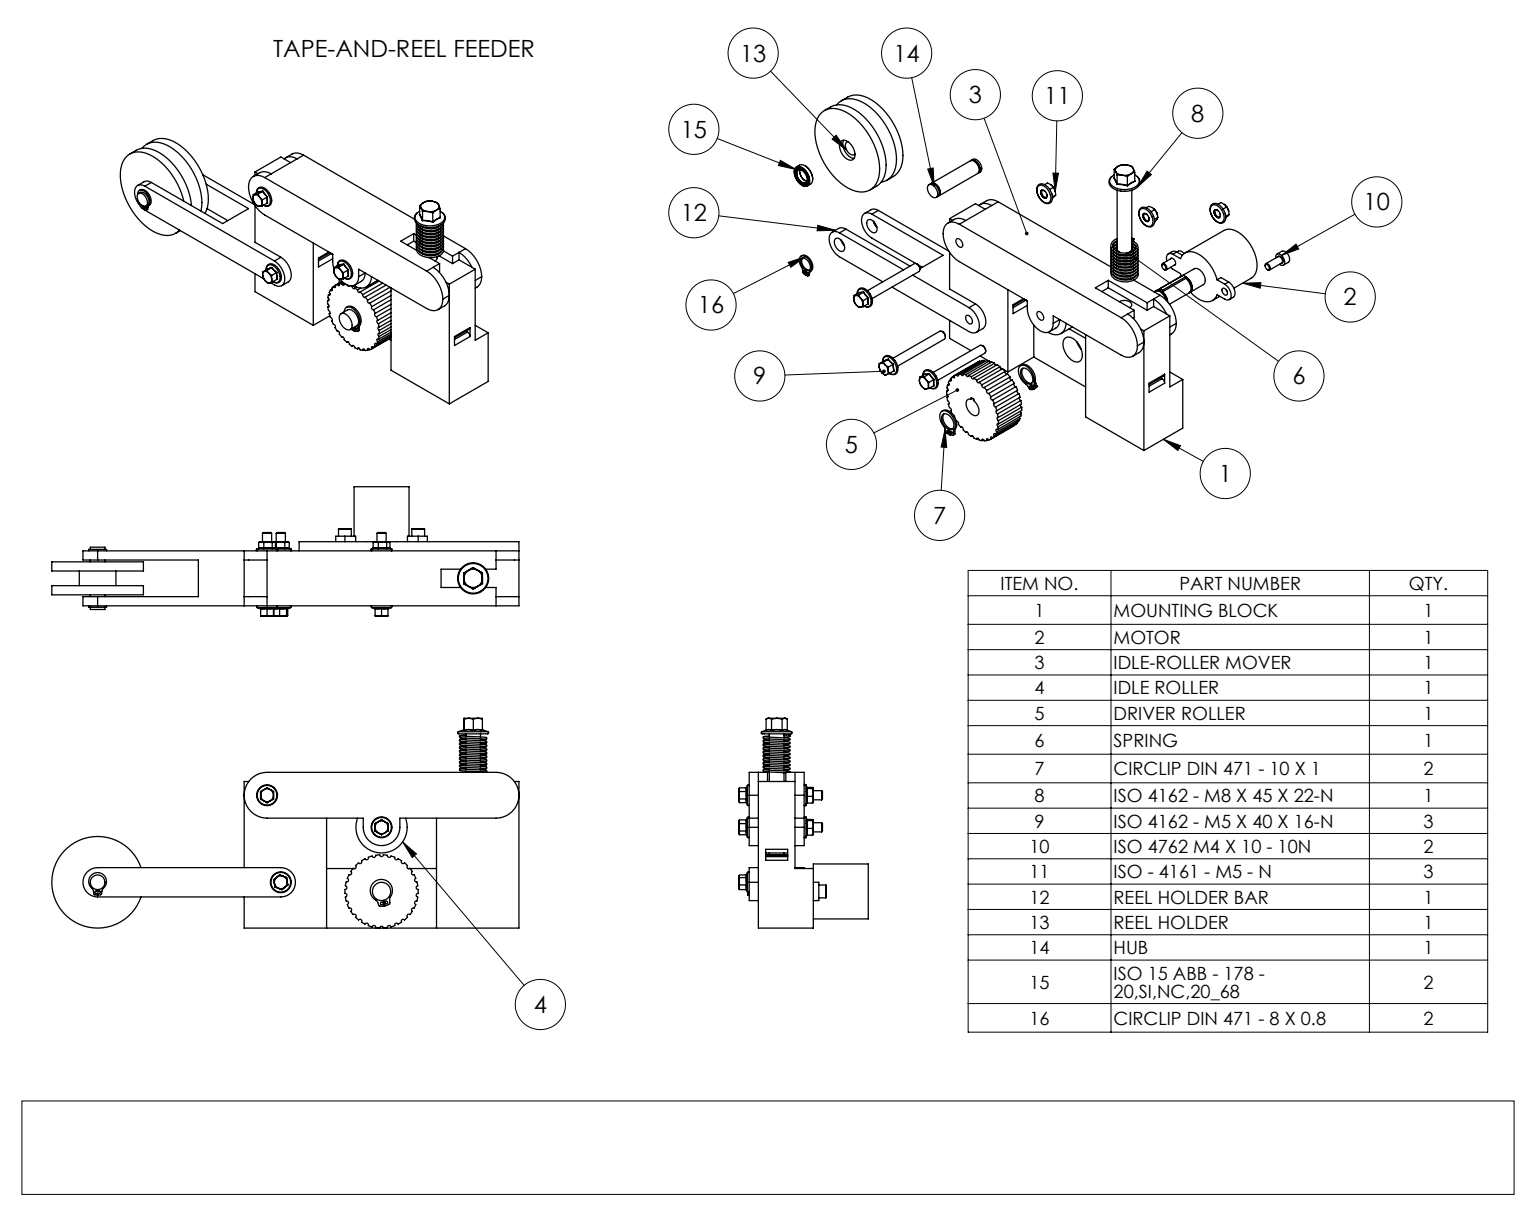
ISO-10303-21;
HEADER;
FILE_DESCRIPTION (('STEP AP214'),
    '1' );
FILE_NAME ('MAS-177',
    '2026-10-31T03:44:21',
    ( '' ),
    ( '' ),
    'SwSTEP 2.0',
    'SolidWorks 2026',
    '' );
FILE_SCHEMA (( 'AUTOMOTIVE_DESIGN' ));
ENDSEC;

DATA;
#1 = CARTESIAN_POINT ( 'NONE',  ( 55.94051828345054389, 59.20051614449765509, 4.345558710429044957 ) ) ;
#2 = ORIENTED_EDGE ( 'NONE', *, *, #6633, .F. ) ;
#3 = DIRECTION ( 'NONE',  ( -0.9999670257950099561, -0.008120795692649453515, 0.000000000000000000 ) ) ;
#4 = CARTESIAN_POINT ( 'NONE',  ( 3.972066048304701891, -2.740530939476090388, 2.384802634787825504 ) ) ;
#5 = CARTESIAN_POINT ( 'NONE',  ( 55.08986747509849380, 53.20051614449766220, 3.727524721679155384 ) ) ;
#6 = CARTESIAN_POINT ( 'NONE',  ( -154.9999999999999716, -14.99999999999999645, 15.00000000000000000 ) ) ;
#7 = CARTESIAN_POINT ( 'NONE',  ( 55.11794222512601493, 60.19948385550240744, 3.688883143319541702 ) ) ;
#8 = DIRECTION ( 'NONE',  ( 0.000000000000000000, 0.000000000000000000, 1.000000000000000000 ) ) ;
#9 = CARTESIAN_POINT ( 'NONE',  ( 44.05948171654949874, 50.79948385550238754, 4.345558710429105354 ) ) ;
#10 = VECTOR ( 'NONE', #15032, 1000.000000000000000 ) ;
#11 = CARTESIAN_POINT ( 'NONE',  ( 43.18075615816994173, 53.80051614449766362, 4.924951120819380357 ) ) ;
#12 = CARTESIAN_POINT ( 'NONE',  ( 6.204460410672268722, -3.831267809382561840, 3.364049496746113199 ) ) ;
#13 = CARTESIAN_POINT ( 'NONE',  ( -57.64999999999994884, -14.99999999999998579, -10.00000000000000178 ) ) ;
#14 = DIRECTION ( 'NONE',  ( -4.082155997157844188E-16, 1.000000000000000000, 0.000000000000000000 ) ) ;
#15 = SURFACE_STYLE_USAGE ( .BOTH. , #11569 ) ;
#16 = SHAPE_DEFINITION_REPRESENTATION ( #10384, #4039 ) ;
#17 = AXIS2_PLACEMENT_3D ( 'NONE', #16816, #16917, #3571 ) ;
#18 = EDGE_LOOP ( 'NONE', ( #11625, #15008, #6307, #1224 ) ) ;
#19 = CARTESIAN_POINT ( 'NONE',  ( 0.000000000000000000, -3.031088913245534755, -1.750000000000001332 ) ) ;
#20 = LINE ( 'NONE', #7849, #12198 ) ;
#21 =( REPRESENTATION_RELATIONSHIP ('NONE','NONE', #16703, #13428 ) REPRESENTATION_RELATIONSHIP_WITH_TRANSFORMATION ( #8023 )SHAPE_REPRESENTATION_RELATIONSHIP( ) );
#22 = AXIS2_PLACEMENT_3D ( 'NONE', #10156, #1151, #17072 ) ;
#23 = CARTESIAN_POINT ( 'NONE',  ( 50.02271294988512551, 62.49948385550240459, 7.000000000000000888 ) ) ;
#24 = VECTOR ( 'NONE', #9487, 1000.000000000000000 ) ;
#25 = CARTESIAN_POINT ( 'NONE',  ( 5.000000000000003553, -20.00000000000000000, 9.999999999999998224 ) ) ;
#26 = CIRCLE ( 'NONE', #5977, 1.999999999999998224 ) ;
#27 = DIRECTION ( 'NONE',  ( -0.000000000000000000, -0.000000000000000000, -1.000000000000000000 ) ) ;
#28 = FACE_OUTER_BOUND ( 'NONE', #18793, .T. ) ;
#29 = CARTESIAN_POINT ( 'NONE',  ( 47.74827507625478518, 56.59948385550238470, 7.007379884777227730 ) ) ;
#30 = CIRCLE ( 'NONE', #4409, 4.100000000000000533 ) ;
#31 = DIRECTION ( 'NONE',  ( -0.000000000000000000, 1.000000000000000000, -0.000000000000000000 ) ) ;
#32 = CARTESIAN_POINT ( 'NONE',  ( 54.68390685589033495, 51.69948385550241454, -6.485486291978119766 ) ) ;
#33 = CARTESIAN_POINT ( 'NONE',  ( 1.150000000000001688, 7.347880794884120722E-16, 6.000000000000000888 ) ) ;
#34 = CARTESIAN_POINT ( 'NONE',  ( 56.65037692655921120, 57.10051614449766078, 2.184720259617097593 ) ) ;
#35 = DIRECTION ( 'NONE',  ( -1.000000000000000000, 0.000000000000000000, 0.000000000000000000 ) ) ;
#36 = ORIENTED_EDGE ( 'NONE', *, *, #18632, .T. ) ;
#37 =( NAMED_UNIT ( * ) PLANE_ANGLE_UNIT ( ) SI_UNIT ( $, .RADIAN. ) );
#38 = VECTOR ( 'NONE', #9468, 1000.000000000000000 ) ;
#39 = AXIS2_PLACEMENT_3D ( 'NONE', #18626, #14180, #9573 ) ;
#40 = VERTEX_POINT ( 'NONE', #10112 ) ;
#41 = AXIS2_PLACEMENT_3D ( 'NONE', #5038, #18489, #12385 ) ;
#42 = CARTESIAN_POINT ( 'NONE',  ( 13.99999999999999822, 0.000000000000000000, 0.000000000000000000 ) ) ;
#43 = ORIENTED_EDGE ( 'NONE', *, *, #11589, .T. ) ;
#44 = CYLINDRICAL_SURFACE ( 'NONE', #13500, 4.799999999999999822 ) ;
#45 = ORIENTED_EDGE ( 'NONE', *, *, #3522, .F. ) ;
#46 = CARTESIAN_POINT ( 'NONE',  ( 2.000000000000005329, -3.464101615137751722, 0.000000000000000000 ) ) ;
#47 = ORIENTED_EDGE ( 'NONE', *, *, #5852, .F. ) ;
#48 = DIRECTION ( 'NONE',  ( 1.000000000000000000, 0.000000000000000000, 0.000000000000000000 ) ) ;
#49 = DIRECTION ( 'NONE',  ( -0.000000000000000000, -0.000000000000000000, -1.000000000000000000 ) ) ;
#50 = EDGE_CURVE ( 'NONE', #8587, #13131, #8250, .T. ) ;
#51 = CARTESIAN_POINT ( 'NONE',  ( 44.28664221472220675, 59.09948385550240602, -1.832500667257165317 ) ) ;
#52 = CARTESIAN_POINT ( 'NONE',  ( -2.000000000000006661, 3.464101615137750834, 0.000000000000000000 ) ) ;
#53 = DIRECTION ( 'NONE',  ( -1.000000000000000000, 0.000000000000000000, 0.000000000000000000 ) ) ;
#54 = VECTOR ( 'NONE', #3678, 1000.000000000000000 ) ;
#55 = CIRCLE ( 'NONE', #4760, 5.000000000000000888 ) ;
#56 = CARTESIAN_POINT ( 'NONE',  ( 49.97728705011495265, 51.50051614449765935, 8.000000000000001776 ) ) ;
#57 = CARTESIAN_POINT ( 'NONE',  ( 53.54508667620424234, 58.70051614449765509, -4.840751629271188961 ) ) ;
#58 = EDGE_CURVE ( 'NONE', #17997, #75, #9295, .T. ) ;
#59 = AXIS2_PLACEMENT_3D ( 'NONE', #5322, #457, #13965 ) ;
#60 = FACE_OUTER_BOUND ( 'NONE', #12914, .T. ) ;
#61 = FACE_OUTER_BOUND ( 'NONE', #9370, .T. ) ;
#62 = VERTEX_POINT ( 'NONE', #14718 ) ;
#63 = ADVANCED_FACE ( 'NONE', ( #9131 ), #4633, .F. ) ;
#64 = ADVANCED_FACE ( 'NONE', ( #5901 ), #7658, .T. ) ;
#65 = ORIENTED_EDGE ( 'NONE', *, *, #19121, .F. ) ;
#66 = DIRECTION ( 'NONE',  ( -1.000000000000000000, 0.000000000000000000, 0.000000000000000000 ) ) ;
#67 = ORIENTED_EDGE ( 'NONE', *, *, #8672, .F. ) ;
#68 = ADVANCED_FACE ( 'NONE', ( #1306 ), #2882, .T. ) ;
#69 = CARTESIAN_POINT ( 'NONE',  ( 44.05948171654949874, 62.79948385550241596, 4.345558710429105354 ) ) ;
#70 = DIRECTION ( 'NONE',  ( -0.9989677110047504582, -0.04542589977017007230, 1.386346192018204258E-14 ) ) ;
#71 = VERTEX_POINT ( 'NONE', #1398 ) ;
#72 = DIRECTION ( 'NONE',  ( -0.000000000000000000, -0.000000000000000000, 1.000000000000000000 ) ) ;
#73 = CARTESIAN_POINT ( 'NONE',  ( 0.9183817310753816798, -24.91493387504114665, 15.00000000000000355 ) ) ;
#74 = CIRCLE ( 'NONE', #18561, 24.99999999999999289 ) ;
#75 = VERTEX_POINT ( 'NONE', #7374 ) ;
#76 = EDGE_LOOP ( 'NONE', ( #8568, #3625 ) ) ;
#77 = CARTESIAN_POINT ( 'NONE',  ( 58.41169779390614281, 45.99948385550240459, -0.02388180880523160798 ) ) ;
#78 = CARTESIAN_POINT ( 'NONE',  ( -62.49999999999997158, 32.50000000000001421, 15.00000000000000000 ) ) ;
#79 = EDGE_CURVE ( 'NONE', #3064, #8689, #14380, .T. ) ;
#80 = CARTESIAN_POINT ( 'NONE',  ( 50.02271294988512551, 56.49948385550240459, 7.000000000000000888 ) ) ;
#81 = FACE_OUTER_BOUND ( 'NONE', #5769, .T. ) ;
#82 = EDGE_CURVE ( 'NONE', #6843, #7000, #17682, .T. ) ;
#83 = CARTESIAN_POINT ( 'NONE',  ( 4.000000000000000000, -2.309401076758516691, -0.4999999999999995559 ) ) ;
#84 = CARTESIAN_POINT ( 'NONE',  ( 43.34962307344078880, 54.10051614449766788, -2.184720259617096705 ) ) ;
#85 = LINE ( 'NONE', #5764, #17678 ) ;
#86 = SURFACE_STYLE_FILL_AREA ( #10453 ) ;
#87 = CARTESIAN_POINT ( 'NONE',  ( -155.0676494111543491, -18.79939778875158396, -15.79999999999999893 ) ) ;
#88 = VERTEX_POINT ( 'NONE', #4235 ) ;
#89 = ORIENTED_EDGE ( 'NONE', *, *, #4960, .T. ) ;
#90 = ORIENTED_EDGE ( 'NONE', *, *, #9609, .F. ) ;
#91 = CARTESIAN_POINT ( 'NONE',  ( 0.000000000000000000, -4.330127018922193649, -2.500000000000000000 ) ) ;
#92 = CARTESIAN_POINT ( 'NONE',  ( 43.20883090819745576, 64.79948385550240175, 4.963592699179006473 ) ) ;
#93 = DIRECTION ( 'NONE',  ( 0.000000000000000000, 0.000000000000000000, -1.000000000000000000 ) ) ;
#94 = EDGE_LOOP ( 'NONE', ( #13981, #857, #13951, #13577 ) ) ;
#95 = DIRECTION ( 'NONE',  ( -1.000000000000000000, 0.000000000000000000, 0.000000000000000000 ) ) ;
#96 = ORIENTED_EDGE ( 'NONE', *, *, #2338, .F. ) ;
#97 = CARTESIAN_POINT ( 'NONE',  ( 42.63976443033212149, 62.00051614449765225, -0.02388180880514948964 ) ) ;
#98 = EDGE_LOOP ( 'NONE', ( #16825, #4410, #16982, #5745 ) ) ;
#99 = DIRECTION ( 'NONE',  ( -1.000000000000000000, 0.000000000000000000, -0.000000000000000000 ) ) ;
#100 = UNCERTAINTY_MEASURE_WITH_UNIT (LENGTH_MEASURE( 1.000000000000000082E-05 ), #14123, 'distance_accuracy_value', 'NONE');
#101 = CARTESIAN_POINT ( 'NONE',  ( -74.99999999999997158, 1.000000000000000000, -5.999999999999998224 ) ) ;
#102 = EDGE_CURVE ( 'NONE', #16449, #12595, #15014, .T. ) ;
#103 = CARTESIAN_POINT ( 'NONE',  ( 55.11794222512599362, 56.80051614449764941, -3.688883143319583446 ) ) ;
#104 = CARTESIAN_POINT ( 'NONE',  ( -62.49999999999997158, 32.50000000000001421, -15.00000000000000000 ) ) ;
#105 = ADVANCED_FACE ( 'NONE', ( #13344 ), #11768, .F. ) ;
#106 = CARTESIAN_POINT ( 'NONE',  ( 49.97728705011488870, 55.49948385550241170, -6.000000000000000888 ) ) ;
#107 = FACE_OUTER_BOUND ( 'NONE', #1049, .T. ) ;
#108 = CARTESIAN_POINT ( 'NONE',  ( 43.20883090819742023, 54.20051614449766220, -4.963592699178938972 ) ) ;
#109 = CARTESIAN_POINT ( 'NONE',  ( 5.991014884144049368, -4.330127018922197202, -2.500000000000000444 ) ) ;
#110 = CARTESIAN_POINT ( 'NONE',  ( 3.961551342853669944, 3.742715940867779700, -0.5174258321190529086 ) ) ;
#111 = ORIENTED_EDGE ( 'NONE', *, *, #1854, .F. ) ;
#112 = CARTESIAN_POINT ( 'NONE',  ( 8.500000000000000000, 0.000000000000000000, 7.900000000000002132 ) ) ;
#113 =( NAMED_UNIT ( * ) SI_UNIT ( $, .STERADIAN. ) SOLID_ANGLE_UNIT ( ) );
#114 = ORIENTED_EDGE ( 'NONE', *, *, #10804, .F. ) ;
#115 = CARTESIAN_POINT ( 'NONE',  ( 0.000000000000000000, 0.000000000000000000, 0.000000000000000000 ) ) ;
#116 = EDGE_CURVE ( 'NONE', #14983, #12413, #19360, .T. ) ;
#117 = DIRECTION ( 'NONE',  ( 0.000000000000000000, 0.000000000000000000, 1.000000000000000000 ) ) ;
#118 = EDGE_CURVE ( 'NONE', #2113, #2665, #16595, .T. ) ;
#119 = CARTESIAN_POINT ( 'NONE',  ( 43.33558569842703179, 65.09948385550239891, -2.141517661632099223 ) ) ;
#120 = CARTESIAN_POINT ( 'NONE',  ( 6.534533895392294234, 2.951347675328725106, 5.111884124469659341 ) ) ;
#121 = CARTESIAN_POINT ( 'NONE',  ( -0.9999999999999995559, -15.10102051443364246, 9.000000000000000000 ) ) ;
#122 = DIRECTION ( 'NONE',  ( -1.000000000000000000, 0.000000000000000000, 0.000000000000000000 ) ) ;
#123 = CARTESIAN_POINT ( 'NONE',  ( 44.03140696652192787, 61.19948385550239323, -4.306917132069425058 ) ) ;
#124 = CARTESIAN_POINT ( 'NONE',  ( 1.411581201560190495E-15, 4.862606272033091592, -3.745885042887436622 ) ) ;
#125 = CARTESIAN_POINT ( 'NONE',  ( 43.18075615816989199, 53.19948385550240744, -4.924951120819313743 ) ) ;
#126 = DIRECTION ( 'NONE',  ( -0.000000000000000000, -0.000000000000000000, -1.000000000000000000 ) ) ;
#127 = CARTESIAN_POINT ( 'NONE',  ( 45.90387839640208512, 54.30051614449765651, -5.676469297603124353 ) ) ;
#128 = DIRECTION ( 'NONE',  ( 0.000000000000000000, -0.000000000000000000, 1.000000000000000000 ) ) ;
#129 = ORIENTED_EDGE ( 'NONE', *, *, #17684, .F. ) ;
#130 = AXIS2_PLACEMENT_3D ( 'NONE', #17222, #3785, #15743 ) ;
#131 = ORIENTED_EDGE ( 'NONE', *, *, #8892, .F. ) ;
#132 = AXIS2_PLACEMENT_3D ( 'NONE', #16115, #16207, #5718 ) ;
#133 = CARTESIAN_POINT ( 'NONE',  ( 6.527192678185834929, 2.941622124011056272, -5.095038975456026797 ) ) ;
#134 = ORIENTED_EDGE ( 'NONE', *, *, #5000, .T. ) ;
#135 = DIRECTION ( 'NONE',  ( -9.710251638871371392E-17, -5.969973981896233748E-17, -1.000000000000000000 ) ) ;
#136 = CARTESIAN_POINT ( 'NONE',  ( 55.96859303347804371, 62.19948385550240744, 4.306917132069425946 ) ) ;
#137 = PLANE ( 'NONE',  #4619 ) ;
#138 = ORIENTED_EDGE ( 'NONE', *, *, #15996, .F. ) ;
#139 = CARTESIAN_POINT ( 'NONE',  ( -0.2500000000000000000, -8.096141056083446585, -1.000000000000000000 ) ) ;
#140 = LINE ( 'NONE', #4756, #15155 ) ;
#141 = CARTESIAN_POINT ( 'NONE',  ( 51.97223112728254790, 58.39948385550241028, 5.992620115222778487 ) ) ;
#142 = DIRECTION ( 'NONE',  ( -0.9781476007338065770, 0.2079116908177552348, 0.000000000000000000 ) ) ;
#143 = DIRECTION ( 'NONE',  ( -0.000000000000000000, -0.000000000000000000, -1.000000000000000000 ) ) ;
#144 = CARTESIAN_POINT ( 'NONE',  ( 45.31609314410960820, 54.30051614449765651, -6.485486291978072693 ) ) ;
#145 = CIRCLE ( 'NONE', #8274, 20.00000000000000000 ) ;
#146 = CARTESIAN_POINT ( 'NONE',  ( 48.07319477248762496, 54.40051614449765793, -6.007379884777208190 ) ) ;
#147 = B_SPLINE_CURVE_WITH_KNOTS ( 'NONE', 3,
 ( #14538, #3778, #12976, #8661, #17507, #4068 ),
 .UNSPECIFIED., .F., .F.,
 ( 4, 2, 4 ),
 ( 0.000000000000000000, 0.0002095117440854730670, 0.0004190234881709461339 ),
 .UNSPECIFIED. ) ;
#148 = CARTESIAN_POINT ( 'NONE',  ( -0.2000000000000000111, -6.997142273814360713, -0.8000000000000000444 ) ) ;
#149 = DIRECTION ( 'NONE',  ( -0.6520673188974834833, 0.7581610723493047432, 1.805535875966851803E-17 ) ) ;
#150 = ORIENTED_EDGE ( 'NONE', *, *, #5080, .F. ) ;
#151 = ORIENTED_EDGE ( 'NONE', *, *, #16122, .F. ) ;
#152 = CARTESIAN_POINT ( 'NONE',  ( 11.75570504584926468, -3.819660112500910198, 9.000000000000000000 ) ) ;
#153 = VERTEX_POINT ( 'NONE', #25 ) ;
#154 = ADVANCED_FACE ( 'NONE', ( #6013 ), #15557, .T. ) ;
#155 = CARTESIAN_POINT ( 'NONE',  ( 54.09612160359786515, 63.69948385550240744, -5.676469297603166098 ) ) ;
#156 = CARTESIAN_POINT ( 'NONE',  ( -99.99999999999997158, -23.00000000000000711, 15.00000000000000000 ) ) ;
#157 = ORIENTED_EDGE ( 'NONE', *, *, #5820, .T. ) ;
#158 = AXIS2_PLACEMENT_3D ( 'NONE', #16967, #16677, #18346 ) ;
#159 = DIRECTION ( 'NONE',  ( 1.000000000000000000, 0.000000000000000000, 0.000000000000000000 ) ) ;
#160 = PRODUCT_DEFINITION ( 'UNKNOWN', '', #4804, #10473 ) ;
#161 = DIRECTION ( 'NONE',  ( 0.000000000000000000, 0.000000000000000000, 1.000000000000000000 ) ) ;
#162 = VERTEX_POINT ( 'NONE', #1595 ) ;
#163 = DIRECTION ( 'NONE',  ( -0.9999670257950099561, -0.008120795692649453515, 0.000000000000000000 ) ) ;
#164 = VERTEX_POINT ( 'NONE', #8741 ) ;
#165 = CARTESIAN_POINT ( 'NONE',  ( 47.37792948025162332, 47.39948385550241028, -7.992620115222770494 ) ) ;
#166 = CARTESIAN_POINT ( 'NONE',  ( 2.899426713160750069, -23.82535289025860337, -8.999999999999996447 ) ) ;
#167 = EDGE_CURVE ( 'NONE', #12421, #12590, #7736, .T. ) ;
#168 = EDGE_CURVE ( 'NONE', #12513, #18552, #6292, .T. ) ;
#169 = CARTESIAN_POINT ( 'NONE',  ( 55.94051828345050836, 55.79948385550238044, -4.345558710429104465 ) ) ;
#170 = DIRECTION ( 'NONE',  ( 0.000000000000000000, -1.000000000000000000, -0.000000000000000000 ) ) ;
#171 = DIRECTION ( 'NONE',  ( -0.000000000000000000, -0.000000000000000000, -1.000000000000000000 ) ) ;
#172 = CARTESIAN_POINT ( 'NONE',  ( 56.66441430157294690, 56.90051614449766504, -2.141517661632166281 ) ) ;
#173 = CARTESIAN_POINT ( 'NONE',  ( 0.000000000000000000, 0.000000000000000000, -0.8000000000000000444 ) ) ;
#174 = ADVANCED_FACE ( 'NONE', ( #9593 ), #15208, .F. ) ;
#175 = DIRECTION ( 'NONE',  ( 1.000000000000000000, 0.000000000000000000, 0.000000000000000000 ) ) ;
#176 = EDGE_CURVE ( 'NONE', #16215, #3087, #11160, .T. ) ;
#177 = DIRECTION ( 'NONE',  ( 0.000000000000000000, 0.000000000000000000, 1.000000000000000000 ) ) ;
#178 = VERTEX_POINT ( 'NONE', #10980 ) ;
#179 = ORIENTED_EDGE ( 'NONE', *, *, #18456, .F. ) ;
#180 = ORIENTED_EDGE ( 'NONE', *, *, #9393, .F. ) ;
#181 = DIRECTION ( 'NONE',  ( 1.000000000000000000, 0.000000000000000000, 0.000000000000000000 ) ) ;
#182 = SURFACE_STYLE_USAGE ( .BOTH. , #380 ) ;
#183 = CIRCLE ( 'NONE', #15507, 5.000000000000000888 ) ;
#184 = EDGE_CURVE ( 'NONE', #2510, #7366, #17139, .T. ) ;
#185 = CARTESIAN_POINT ( 'NONE',  ( 57.61547081786812896, 64.09948385550239891, 2.450534656007040901 ) ) ;
#186 = EDGE_CURVE ( 'NONE', #9539, #16928, #1996, .T. ) ;
#187 = ORIENTED_EDGE ( 'NONE', *, *, #1986, .T. ) ;
#188 = CARTESIAN_POINT ( 'NONE',  ( -20.63749999999999574, 0.000000000000000000, 0.000000000000000000 ) ) ;
#189 = VERTEX_POINT ( 'NONE', #16887 ) ;
#190 = CARTESIAN_POINT ( 'NONE',  ( 44.05948171654945611, 58.20051614449764799, -4.345558710429044069 ) ) ;
#191 = ORIENTED_EDGE ( 'NONE', *, *, #16975, .F. ) ;
#192 = ADVANCED_FACE ( 'NONE', ( #13732 ), #15592, .F. ) ;
#193 = CARTESIAN_POINT ( 'NONE',  ( -3.158233816355059620, -39.56295201467614220, -9.000000000000000000 ) ) ;
#194 = DIRECTION ( 'NONE',  ( -1.000000000000000000, -0.000000000000000000, -0.000000000000000000 ) ) ;
#195 = EDGE_CURVE ( 'NONE', #14529, #9351, #3542, .T. ) ;
#196 = CARTESIAN_POINT ( 'NONE',  ( 50.02271294988506156, 56.50051614449767357, -6.000000000000000888 ) ) ;
#197 = CARTESIAN_POINT ( 'NONE',  ( 0.000000000000000000, 4.163799117101000559E-16, -3.299999999999999822 ) ) ;
#198 = CIRCLE ( 'NONE', #9874, 1.000000000000000000 ) ;
#199 = CARTESIAN_POINT ( 'NONE',  ( -19.30627432446647163, -14.77814480204146363, 9.000000000000000000 ) ) ;
#200 = CARTESIAN_POINT ( 'NONE',  ( 46.49166364869460466, 56.69948385550240744, 4.867452303228209765 ) ) ;
#201 = CARTESIAN_POINT ( 'NONE',  ( 2.000000000000000000, 1.773042676681340524, -2.059984127722458425E-15 ) ) ;
#202 = CARTESIAN_POINT ( 'NONE',  ( 47.37792948025170858, 53.60051614449765367, 7.992620115222797139 ) ) ;
#203 = DIRECTION ( 'NONE',  ( -0.000000000000000000, -0.000000000000000000, 1.000000000000000000 ) ) ;
#204 = CARTESIAN_POINT ( 'NONE',  ( -4.204015924366189871, 1.626724848190922446, -3.610627190413390419 ) ) ;
#205 = AXIS2_PLACEMENT_3D ( 'NONE', #2952, #1472, #19344 ) ;
#206 = VERTEX_POINT ( 'NONE', #16694 ) ;
#207 = CARTESIAN_POINT ( 'NONE',  ( 5.599999999999999645, 0.000000000000000000, 0.000000000000000000 ) ) ;
#208 = APPLICATION_PROTOCOL_DEFINITION ( 'draft international standard', 'automotive_design', 1998, #2406 ) ;
#209 = ORIENTED_EDGE ( 'NONE', *, *, #14535, .T. ) ;
#210 = CARTESIAN_POINT ( 'NONE',  ( -1.398397006336996817, -6.091550361990593743, -0.8000000000000000444 ) ) ;
#211 = DIRECTION ( 'NONE',  ( -0.000000000000000000, -0.000000000000000000, 1.000000000000000000 ) ) ;
#212 = CARTESIAN_POINT ( 'NONE',  ( 55.96859303347805081, 62.19948385550241454, 4.306917132069425058 ) ) ;
#213 = DIRECTION ( 'NONE',  ( -1.000000000000000000, -0.000000000000000000, 0.000000000000000000 ) ) ;
#214 = DIRECTION ( 'NONE',  ( -0.000000000000000000, 0.000000000000000000, 1.000000000000000000 ) ) ;
#215 = CYLINDRICAL_SURFACE ( 'NONE', #17154, 2.447112362156698140 ) ;
#216 = CARTESIAN_POINT ( 'NONE',  ( 56.65037692655918988, 57.89948385550240317, -2.184720259617163762 ) ) ;
#217 = DIRECTION ( 'NONE',  ( 0.000000000000000000, 0.000000000000000000, 1.000000000000000000 ) ) ;
#218 = CIRCLE ( 'NONE', #11155, 4.799999999999999822 ) ;
#219 = CARTESIAN_POINT ( 'NONE',  ( 52.57664461997811856, 55.59948385550240602, -8.007379884777229506 ) ) ;
#220 = DIRECTION ( 'NONE',  ( 0.000000000000000000, 0.000000000000000000, -1.000000000000000000 ) ) ;
#221 = CARTESIAN_POINT ( 'NONE',  ( 47.74827507625469281, 54.40051614449766504, -7.007379884777203749 ) ) ;
#222 = EDGE_CURVE ( 'NONE', #2993, #6110, #13306, .T. ) ;
#223 = DIRECTION ( 'NONE',  ( 2.191393683118470056E-17, 7.538405132783724027E-17, 1.000000000000000000 ) ) ;
#224 = ADVANCED_FACE ( 'NONE', ( #6567 ), #9413, .T. ) ;
#225 = ORIENTED_EDGE ( 'NONE', *, *, #17454, .F. ) ;
#226 = VECTOR ( 'NONE', #4356, 1000.000000000000000 ) ;
#227 = DIRECTION ( 'NONE',  ( 0.000000000000000000, -0.000000000000000000, 1.000000000000000000 ) ) ;
#228 = VERTEX_POINT ( 'NONE', #12449 ) ;
#229 = CARTESIAN_POINT ( 'NONE',  ( 57.36023556966787851, 49.00051614449764514, 0.02388180880515038476 ) ) ;
#230 = CARTESIAN_POINT ( 'NONE',  ( 50.02271294988512551, 62.49948385550240459, 7.000000000000000888 ) ) ;
#231 = DIRECTION ( 'NONE',  ( 1.000000000000000000, 0.000000000000000000, 0.000000000000000000 ) ) ;
#232 = EDGE_LOOP ( 'NONE', ( #13470, #855 ) ) ;
#233 = DIRECTION ( 'NONE',  ( -0.3090169943749528914, 0.9510565162951518658, 0.000000000000000000 ) ) ;
#234 = DIRECTION ( 'NONE',  ( 0.000000000000000000, 0.000000000000000000, 1.000000000000000000 ) ) ;
#235 = CARTESIAN_POINT ( 'NONE',  ( 44.91013252490152752, 56.79948385550240175, 3.727524721679198461 ) ) ;
#236 = PLANE ( 'NONE',  #7905 ) ;
#237 = PRESENTATION_STYLE_ASSIGNMENT (( #8960 ) ) ;
#238 = AXIS2_PLACEMENT_3D ( 'NONE', #6880, #15913, #19069 ) ;
#239 = CARTESIAN_POINT ( 'NONE',  ( 49.97728705011495265, 55.50051614449766646, 8.000000000000001776 ) ) ;
#240 = CARTESIAN_POINT ( 'NONE',  ( 53.50833635130544508, 57.30051614449767072, 4.867452303228181343 ) ) ;
#241 = AXIS2_PLACEMENT_3D ( 'NONE', #17266, #3826, #15783 ) ;
#242 = FACE_OUTER_BOUND ( 'NONE', #17390, .T. ) ;
#243 = VECTOR ( 'NONE', #1548, 1000.000000000000114 ) ;
#244 = CARTESIAN_POINT ( 'NONE',  ( 22.14999999999999858, -20.00000000000000000, -20.00000000000000000 ) ) ;
#245 = ORIENTED_EDGE ( 'NONE', *, *, #9904, .T. ) ;
#246 = ORIENTED_EDGE ( 'NONE', *, *, #5677, .F. ) ;
#247 = CARTESIAN_POINT ( 'NONE',  ( 6.327625087026996553, 2.033113452595566972, -4.999999999998725464 ) ) ;
#248 = VERTEX_POINT ( 'NONE', #13911 ) ;
#249 = DIRECTION ( 'NONE',  ( -9.710251638871371392E-17, -5.969973981896233748E-17, -1.000000000000000000 ) ) ;
#250 = DIRECTION ( 'NONE',  ( 0.000000000000000000, 0.000000000000000000, 1.000000000000000000 ) ) ;
#251 = CIRCLE ( 'NONE', #8059, 3.800000000000000266 ) ;
#252 = ORIENTED_EDGE ( 'NONE', *, *, #14423, .F. ) ;
#253 = DIRECTION ( 'NONE',  ( 1.000000000000000000, 0.000000000000000000, 0.000000000000000000 ) ) ;
#254 = CARTESIAN_POINT ( 'NONE',  ( 55.94051828345050836, 51.79948385550240175, -4.345558710429103577 ) ) ;
#255 = CONICAL_SURFACE ( 'NONE', #13715, 2.055000000000000160, 0.7853981633974400633 ) ;
#256 = ORIENTED_EDGE ( 'NONE', *, *, #7357, .T. ) ;
#257 = DIRECTION ( 'NONE',  ( 0.1836763462126260738, -0.9829867750086873635, -1.521953536530129477E-22 ) ) ;
#258 = VERTEX_POINT ( 'NONE', #12266 ) ;
#259 = CARTESIAN_POINT ( 'NONE',  ( 56.81924384183011512, 48.19948385550240744, 4.924951120819313743 ) ) ;
#260 = CARTESIAN_POINT ( 'NONE',  ( 9.999999999999994671, 20.00000000000001421, -9.999999999999998224 ) ) ;
#261 = CARTESIAN_POINT ( 'NONE',  ( 52.25172492374522903, 57.59948385550241312, -7.007379884777225953 ) ) ;
#262 = CARTESIAN_POINT ( 'NONE',  ( -154.9999999999999716, -14.99999999999999645, 15.79999999999999893 ) ) ;
#263 =( GEOMETRIC_REPRESENTATION_CONTEXT ( 3 ) GLOBAL_UNCERTAINTY_ASSIGNED_CONTEXT ( ( #6357 ) ) GLOBAL_UNIT_ASSIGNED_CONTEXT ( ( #5384, #15479, #3919 ) ) REPRESENTATION_CONTEXT ( 'NONE', 'WORKASPACE' ) );
#264 = CARTESIAN_POINT ( 'NONE',  ( 54.09612160359792199, 57.30051614449765651, 5.676469297603124353 ) ) ;
#265 = EDGE_CURVE ( 'NONE', #12240, #6347, #18266, .T. ) ;
#266 = CYLINDRICAL_SURFACE ( 'NONE', #9428, 5.999999999999977796 ) ;
#267 = CARTESIAN_POINT ( 'NONE',  ( 6.452281807715811723, -5.797857616945994330, 1.289641217033754180E-15 ) ) ;
#268 = ORIENTED_EDGE ( 'NONE', *, *, #16061, .T. ) ;
#269 = AXIS2_PLACEMENT_3D ( 'NONE', #14296, #874, #6847 ) ;
#270 = CONICAL_SURFACE ( 'NONE', #1210, 5.000000000000000000, 1.047197551196600296 ) ;
#271 = ORIENTED_EDGE ( 'NONE', *, *, #6050, .F. ) ;
#272 =( REPRESENTATION_RELATIONSHIP ('NONE','NONE', #16703, #1297 ) REPRESENTATION_RELATIONSHIP_WITH_TRANSFORMATION ( #5475 )SHAPE_REPRESENTATION_RELATIONSHIP( ) );
#273 = VERTEX_POINT ( 'NONE', #10784 ) ;
#274 = DIRECTION ( 'NONE',  ( -0.6691306063588506881, -0.7431448254774009055, 0.000000000000000000 ) ) ;
#275 =( NAMED_UNIT ( * ) PLANE_ANGLE_UNIT ( ) SI_UNIT ( $, .RADIAN. ) );
#276 = CARTESIAN_POINT ( 'NONE',  ( 55.94051828345050836, 45.79948385550240886, -4.345558710429104465 ) ) ;
#277 = DIRECTION ( 'NONE',  ( 1.000000000000000000, 0.000000000000000000, 0.000000000000000000 ) ) ;
#278 = COLOUR_RGB ( '',0.8941176470588234615, 0.8941176470588234615, 0.8941176470588234615 ) ;
#279 = ORIENTED_EDGE ( 'NONE', *, *, #12618, .T. ) ;
#280 = DIRECTION ( 'NONE',  ( 1.000000000000000000, 0.000000000000000000, 0.000000000000000000 ) ) ;
#281 = EDGE_CURVE ( 'NONE', #8618, #8760, #1727, .T. ) ;
#282 = ORIENTED_EDGE ( 'NONE', *, *, #2242, .F. ) ;
#283 = CARTESIAN_POINT ( 'NONE',  ( 43.33558569842706021, 59.90051614449766504, 2.141517661632167169 ) ) ;
#284 = ORIENTED_EDGE ( 'NONE', *, *, #7843, .F. ) ;
#285 = AXIS2_PLACEMENT_3D ( 'NONE', #12614, #3232, #18241 ) ;
#286 = AXIS2_PLACEMENT_3D ( 'NONE', #15850, #18712, #8496 ) ;
#287 = DIRECTION ( 'NONE',  ( -0.000000000000000000, 0.000000000000000000, -1.000000000000000000 ) ) ;
#288 = UNCERTAINTY_MEASURE_WITH_UNIT (LENGTH_MEASURE( 1.000000000000000082E-05 ), #7865, 'distance_accuracy_value', 'NONE');
#289 = DIRECTION ( 'NONE',  ( -0.000000000000000000, -0.000000000000000000, -1.000000000000000000 ) ) ;
#290 = CARTESIAN_POINT ( 'NONE',  ( 44.30067958973594955, 54.10051614449766078, -1.875703265242155693 ) ) ;
#291 = DIRECTION ( 'NONE',  ( 1.000000000000000000, 0.000000000000000000, 0.000000000000000000 ) ) ;
#292 = ADVANCED_FACE ( 'NONE', ( #12553 ), #11732, .T. ) ;
#293 = CARTESIAN_POINT ( 'NONE',  ( 0.000000000000000000, 3.061616997868383634E-16, -2.500000000000000444 ) ) ;
#294 = EDGE_CURVE ( 'NONE', #606, #16278, #14874, .T. ) ;
#295 = EDGE_CURVE ( 'NONE', #1806, #3807, #8927, .T. ) ;
#296 = CARTESIAN_POINT ( 'NONE',  ( 48.02776887271745210, 61.39948385550240317, -5.992620115222778487 ) ) ;
#297 = AXIS2_PLACEMENT_3D ( 'NONE', #11175, #5302, #12659 ) ;
#298 = CARTESIAN_POINT ( 'NONE',  ( 2.000000000000000000, 0.000000000000000000, 1.535500000000000087 ) ) ;
#299 = CARTESIAN_POINT ( 'NONE',  ( 47.37792948025170858, 55.60051614449765367, 7.992620115222797139 ) ) ;
#300 = FACE_OUTER_BOUND ( 'NONE', #17953, .T. ) ;
#301 = EDGE_CURVE ( 'NONE', #4092, #18359, #6415, .T. ) ;
#302 = EDGE_LOOP ( 'NONE', ( #1176, #3986, #11938, #3229 ) ) ;
#303 = DIRECTION ( 'NONE',  ( 0.000000000000000000, 0.000000000000000000, 1.000000000000000000 ) ) ;
#304 = FILL_AREA_STYLE_COLOUR ( '', #11512 ) ;
#305 = AXIS2_PLACEMENT_3D ( 'NONE', #18598, #17407, #12786 ) ;
#307 = ORIENTED_EDGE ( 'NONE', *, *, #12740, .F. ) ;
#306 = EDGE_CURVE ( 'NONE', #15034, #6054, #602, .T. ) ;
#308 = CIRCLE ( 'NONE', #3740, 12.49999999999999645 ) ;
#309 = DIRECTION ( 'NONE',  ( -0.000000000000000000, -0.000000000000000000, -1.000000000000000000 ) ) ;
#310 = ORIENTED_EDGE ( 'NONE', *, *, #4548, .T. ) ;
#311 = DIRECTION ( 'NONE',  ( 1.000000000000000000, -0.000000000000000000, 0.000000000000000000 ) ) ;
#312 = DIRECTION ( 'NONE',  ( 1.000000000000000000, 0.000000000000000000, 0.000000000000000000 ) ) ;
#313 = CIRCLE ( 'NONE', #4397, 1.000000000000000444 ) ;
#314 = DIRECTION ( 'NONE',  ( -1.000000000000000000, -0.000000000000000000, -0.000000000000000000 ) ) ;
#315 = DIRECTION ( 'NONE',  ( -1.000000000000000000, 0.000000000000000000, 0.000000000000000000 ) ) ;
#316 = AXIS2_PLACEMENT_3D ( 'NONE', #4750, #1802, #7770 ) ;
#317 = DIRECTION ( 'NONE',  ( 0.000000000000000000, 0.000000000000000000, 1.000000000000000000 ) ) ;
#318 = ADVANCED_FACE ( 'NONE', ( #14500 ), #9696, .T. ) ;
#319 = DIRECTION ( 'NONE',  ( 0.8191520442889902442, 1.003171929053522651E-16, -0.5735764363510482688 ) ) ;
#320 = EDGE_CURVE ( 'NONE', #4165, #8587, #2277, .T. ) ;
#321 = CARTESIAN_POINT ( 'NONE',  ( 49.97728705011488159, 55.49948385550240459, -7.000000000000000888 ) ) ;
#322 = DIRECTION ( 'NONE',  ( 0.000000000000000000, 0.000000000000000000, -1.000000000000000000 ) ) ;
#323 = CARTESIAN_POINT ( 'NONE',  ( 47.37792948025162332, 57.39948385550241028, -7.992620115222770494 ) ) ;
#324 = CARTESIAN_POINT ( 'NONE',  ( 47.74827507625469281, 52.40051614449763662, -7.007379884777203749 ) ) ;
#325 = AXIS2_PLACEMENT_3D ( 'NONE', #12478, #15527, #6324 ) ;
#326 = DIRECTION ( 'NONE',  ( 1.000000000000000000, 0.000000000000000000, 0.000000000000000000 ) ) ;
#327 = CARTESIAN_POINT ( 'NONE',  ( 0.000000000000000000, 0.000000000000000000, -9.000000000000000000 ) ) ;
#328 = FILL_AREA_STYLE_COLOUR ( '', #15956 ) ;
#329 = ORIENTED_EDGE ( 'NONE', *, *, #6092, .T. ) ;
#330 = LINE ( 'NONE', #424, #19101 ) ;
#331 = CIRCLE ( 'NONE', #9396, 2.500000000000000444 ) ;
#332 = AXIS2_PLACEMENT_3D ( 'NONE', #14150, #12396, #6331 ) ;
#333 = FACE_OUTER_BOUND ( 'NONE', #13418, .T. ) ;
#334 = CARTESIAN_POINT ( 'NONE',  ( 54.13287192849676188, 64.29948385550241596, 5.649768623646098220 ) ) ;
#335 = CIRCLE ( 'NONE', #6899, 4.000000000000003553 ) ;
#336 = DIRECTION ( 'NONE',  ( -0.8660254037844373753, 0.5000000000000021094, 0.000000000000000000 ) ) ;
#337 = VERTEX_POINT ( 'NONE', #4121 ) ;
#338 = CARTESIAN_POINT ( 'NONE',  ( -1.150000000000001688, 0.000000000000000000, -6.000000000000001776 ) ) ;
#339 = DIRECTION ( 'NONE',  ( 1.000000000000000000, -0.000000000000000000, -0.000000000000000000 ) ) ;
#340 = EDGE_CURVE ( 'NONE', #6420, #12615, #2499, .T. ) ;
#341 = CARTESIAN_POINT ( 'NONE',  ( 46.49166364869460466, 60.69948385550240033, 4.867452303228209765 ) ) ;
#342 = FACE_OUTER_BOUND ( 'NONE', #4754, .T. ) ;
#343 = CARTESIAN_POINT ( 'NONE',  ( -99.99999999999997158, -23.00000000000000711, -15.00000000000000000 ) ) ;
#344 = EDGE_CURVE ( 'NONE', #16928, #11423, #12506, .T. ) ;
#345 = CARTESIAN_POINT ( 'NONE',  ( 43.18075615816994173, 57.80051614449766362, 4.924951120819380357 ) ) ;
#346 = CARTESIAN_POINT ( 'NONE',  ( 49.97728705011494554, 57.50051614449766646, 6.000000000000000888 ) ) ;
#347 = EDGE_CURVE ( 'NONE', #6641, #7321, #477, .T. ) ;
#349 = CONICAL_SURFACE ( 'NONE', #11281, 5.371010071662833063, 1.221730476396037490 ) ;
#348 = DIRECTION ( 'NONE',  ( -0.000000000000000000, -0.000000000000000000, -1.000000000000000000 ) ) ;
#350 = AXIS2_PLACEMENT_3D ( 'NONE', #1219, #5627, #11312 ) ;
#351 = CARTESIAN_POINT ( 'NONE',  ( -154.9999999999999716, -14.99999999999999645, -6.499999999999999112 ) ) ;
#352 = ORIENTED_EDGE ( 'NONE', *, *, #9202, .F. ) ;
#353 = AXIS2_PLACEMENT_3D ( 'NONE', #12946, #2182, #2381 ) ;
#354 = ORIENTED_EDGE ( 'NONE', *, *, #1026, .F. ) ;
#355 = DIRECTION ( 'NONE',  ( 0.000000000000000000, 0.000000000000000000, -1.000000000000000000 ) ) ;
#356 = ORIENTED_EDGE ( 'NONE', *, *, #17810, .F. ) ;
#357 = DIRECTION ( 'NONE',  ( 0.000000000000000000, 0.000000000000000000, -1.000000000000000000 ) ) ;
#358 = ORIENTED_EDGE ( 'NONE', *, *, #8483, .F. ) ;
#359 = DIRECTION ( 'NONE',  ( -0.000000000000000000, 1.000000000000000000, -0.000000000000000000 ) ) ;
#360 = CARTESIAN_POINT ( 'NONE',  ( 52.25172492374522903, 49.59948385550240602, -7.007379884777227730 ) ) ;
#361 = EDGE_CURVE ( 'NONE', #6066, #19035, #785, .T. ) ;
#362 = ORIENTED_EDGE ( 'NONE', *, *, #7302, .F. ) ;
#363 = CARTESIAN_POINT ( 'NONE',  ( -2.000000000000006661, 3.464101615137750834, 0.000000000000000000 ) ) ;
#364 = AXIS2_PLACEMENT_3D ( 'NONE', #11139, #15465, #17247 ) ;
#365 = EDGE_LOOP ( 'NONE', ( #11138, #12423, #1460, #7331 ) ) ;
#366 = CARTESIAN_POINT ( 'NONE',  ( 54.72065718078924590, 46.29948385550240886, 6.458785618021043895 ) ) ;
#367 = AXIS2_PLACEMENT_3D ( 'NONE', #6405, #16916, #9445 ) ;
#368 = FACE_OUTER_BOUND ( 'NONE', #2307, .T. ) ;
#369 = ADVANCED_FACE ( 'NONE', ( #6760 ), #18743, .T. ) ;
#370 = CARTESIAN_POINT ( 'NONE',  ( 56.66441430157296821, 64.09948385550239891, 2.141517661632100111 ) ) ;
#371 = DIRECTION ( 'NONE',  ( 1.000000000000000000, 0.000000000000000000, 0.000000000000000000 ) ) ;
#372 =( NAMED_UNIT ( * ) SI_UNIT ( $, .STERADIAN. ) SOLID_ANGLE_UNIT ( ) );
#373 = CARTESIAN_POINT ( 'NONE',  ( 47.74827507625469281, 56.40051614449766504, -7.007379884777203749 ) ) ;
#374 = B_SPLINE_CURVE_WITH_KNOTS ( 'NONE', 3,
 ( #17934, #13506, #10742, #16839, #1743, #16743 ),
 .UNSPECIFIED., .F., .F.,
 ( 4, 2, 4 ),
 ( 0.000000000000000000, 0.001488912493401906576, 0.002977824986803813152 ),
 .UNSPECIFIED. ) ;
#375 = CARTESIAN_POINT ( 'NONE',  ( 52.25172492374522903, 53.59948385550241312, -7.007379884777225953 ) ) ;
#376 = DIRECTION ( 'NONE',  ( -0.000000000000000000, -0.000000000000000000, 1.000000000000000000 ) ) ;
#377 = ORIENTED_EDGE ( 'NONE', *, *, #16114, .F. ) ;
#378 = ORIENTED_EDGE ( 'NONE', *, *, #13840, .F. ) ;
#379 = CARTESIAN_POINT ( 'NONE',  ( -1.398397006336996817, -6.091550361990593743, -0.8000000000000000444 ) ) ;
#380 = SURFACE_SIDE_STYLE ('',( #4792 ) ) ;
#381 = CARTESIAN_POINT ( 'NONE',  ( 56.66441430157296821, 54.09948385550240602, 2.141517661632100111 ) ) ;
#382 = AXIS2_PLACEMENT_3D ( 'NONE', #14726, #11588, #19073 ) ;
#383 = DIRECTION ( 'NONE',  ( 0.000000000000000000, 0.000000000000000000, 1.000000000000000000 ) ) ;
#384 = ORIENTED_EDGE ( 'NONE', *, *, #11180, .F. ) ;
#385 = FACE_OUTER_BOUND ( 'NONE', #2616, .T. ) ;
#386 = ORIENTED_EDGE ( 'NONE', *, *, #1313, .F. ) ;
#387 = CARTESIAN_POINT ( 'NONE',  ( 47.70284917648459810, 59.60051614449765367, 6.992620115222797139 ) ) ;
#388 = ORIENTED_EDGE ( 'NONE', *, *, #14666, .F. ) ;
#389 = CARTESIAN_POINT ( 'NONE',  ( 1.828356344711641102, 3.563200125723180900, -5.433716356636336675E-16 ) ) ;
#390 = CYLINDRICAL_SURFACE ( 'NONE', #7746, 1.999999999999998224 ) ;
#391 = CARTESIAN_POINT ( 'NONE',  ( 46.45491332379576477, 55.70051614449766220, 4.840751629271188961 ) ) ;
#392 = DIRECTION ( 'NONE',  ( 0.000000000000000000, 0.000000000000000000, -1.000000000000000000 ) ) ;
#393 = DIRECTION ( 'NONE',  ( -0.000000000000000000, -0.000000000000000000, -1.000000000000000000 ) ) ;
#394 = CARTESIAN_POINT ( 'NONE',  ( 53.50833635130540955, 61.69948385550240744, -4.867452303228209765 ) ) ;
#395 = CARTESIAN_POINT ( 'NONE',  ( 6.371506350351443970, 3.439339428956429856, -4.260454149911179655 ) ) ;
#396 = CARTESIAN_POINT ( 'NONE',  ( 47.37792948025170858, 57.60051614449765367, 7.992620115222797139 ) ) ;
#397 = ORIENTED_EDGE ( 'NONE', *, *, #12870, .T. ) ;
#398 = DIRECTION ( 'NONE',  ( 0.000000000000000000, 0.000000000000000000, 1.000000000000000000 ) ) ;
#399 =( LENGTH_UNIT ( ) NAMED_UNIT ( * ) SI_UNIT ( .MILLI., .METRE. ) );
#400 = ORIENTED_EDGE ( 'NONE', *, *, #7836, .F. ) ;
#401 = AXIS2_PLACEMENT_3D ( 'NONE', #6427, #3787, #15746 ) ;
#402 = VERTEX_POINT ( 'NONE', #17273 ) ;
#403 = DIRECTION ( 'NONE',  ( 0.000000000000000000, 0.000000000000000000, -1.000000000000000000 ) ) ;
#404 = EDGE_CURVE ( 'NONE', #12345, #17767, #17395, .T. ) ;
#405 = CARTESIAN_POINT ( 'NONE',  ( 4.050823680195224874, 3.779313952391379239, -0.5899027668435166127 ) ) ;
#406 = EDGE_CURVE ( 'NONE', #12668, #6480, #5479, .T. ) ;
#407 = CARTESIAN_POINT ( 'NONE',  ( 47.70284917648453415, 65.39948385550239607, -6.992620115222774047 ) ) ;
#408 = DIRECTION ( 'NONE',  ( 0.000000000000000000, 0.000000000000000000, 1.000000000000000000 ) ) ;
#409 = PLANE ( 'NONE',  #5457 ) ;
#410 = ADVANCED_FACE ( 'NONE', ( #9796 ), #12997, .T. ) ;
#411 = ADVANCED_FACE ( 'NONE', ( #6668, #2372, #8326 ), #18944, .F. ) ;
#412 = CARTESIAN_POINT ( 'NONE',  ( -54.99999999999996447, -14.99999999999998579, -10.00000000000000178 ) ) ;
#413 = CARTESIAN_POINT ( 'NONE',  ( 56.66441430157296821, 62.09948385550239891, 2.141517661632100111 ) ) ;
#414 = CARTESIAN_POINT ( 'NONE',  ( 4.071447262713887127, 2.020725942163688504, 3.500000000000000000 ) ) ;
#415 = CARTESIAN_POINT ( 'NONE',  ( 54.72065718078924590, 62.29948385550241596, 6.458785618021043895 ) ) ;
#416 = CARTESIAN_POINT ( 'NONE',  ( 57.36023556966787851, 63.00051614449767357, 0.02388180880515038476 ) ) ;
#417 = EDGE_CURVE ( 'NONE', #1879, #10892, #2680, .T. ) ;
#418 = AXIS2_PLACEMENT_3D ( 'NONE', #11692, #1217, #13364 ) ;
#419 = CARTESIAN_POINT ( 'NONE',  ( -2.141980652367355020, -6.189445006155633422, 0.000000000000000000 ) ) ;
#420 = DIRECTION ( 'NONE',  ( 0.000000000000000000, 0.000000000000000000, -1.000000000000000000 ) ) ;
#421 = ORIENTED_EDGE ( 'NONE', *, *, #11100, .F. ) ;
#422 = EDGE_CURVE ( 'NONE', #7933, #6445, #10544, .T. ) ;
#423 = EDGE_CURVE ( 'NONE', #3823, #976, #17703, .T. ) ;
#424 = CARTESIAN_POINT ( 'NONE',  ( -158.9999999999999716, -14.99999999999999645, 15.00000000000000000 ) ) ;
#425 = CARTESIAN_POINT ( 'NONE',  ( 44.03140696652198471, 45.80051614449766362, 4.306917132069485454 ) ) ;
#426 = CARTESIAN_POINT ( 'NONE',  ( 55.96859303347804371, 64.19948385550239323, 4.306917132069425946 ) ) ;
#427 = DIRECTION ( 'NONE',  ( -9.710251638871371392E-17, -5.969973981896233748E-17, -1.000000000000000000 ) ) ;
#428 = ORIENTED_EDGE ( 'NONE', *, *, #9768, .T. ) ;
#429 = DIRECTION ( 'NONE',  ( -0.000000000000000000, -0.000000000000000000, 1.000000000000000000 ) ) ;
#430 = CYLINDRICAL_SURFACE ( 'NONE', #1391, 4.599999999999999645 ) ;
#431 = CARTESIAN_POINT ( 'NONE',  ( 43.69122665457040000, 64.99948385550240459, 0.02388180880521036456 ) ) ;
#432 = DIRECTION ( 'NONE',  ( 0.000000000000000000, 0.000000000000000000, 1.000000000000000000 ) ) ;
#433 = CARTESIAN_POINT ( 'NONE',  ( 42.38452918213190657, 61.90051614449766504, 2.450534656007115508 ) ) ;
#434 = CARTESIAN_POINT ( 'NONE',  ( 44.88205777487401349, 57.80051614449766362, 3.688883143319584779 ) ) ;
#435 = VECTOR ( 'NONE', #5633, 1000.000000000000000 ) ;
#436 = CARTESIAN_POINT ( 'NONE',  ( 1.000000000000000000, -5.408326913195983465, -0.8000000000000000444 ) ) ;
#437 = DIRECTION ( 'NONE',  ( 0.000000000000000000, 0.000000000000000000, 1.000000000000000000 ) ) ;
#438 = CIRCLE ( 'NONE', #9207, 1.000000000000000222 ) ;
#439 = VERTEX_POINT ( 'NONE', #4586 ) ;
#440 = VERTEX_POINT ( 'NONE', #7521 ) ;
#441 = CARTESIAN_POINT ( 'NONE',  ( 75.00000000000000000, 40.00000000000000000, 10.00000000000000000 ) ) ;
#442 = VERTEX_POINT ( 'NONE', #8621 ) ;
#443 = CARTESIAN_POINT ( 'NONE',  ( 4.175813232069150338, -4.122719923832746325, 2.362127131240695889E-16 ) ) ;
#444 = VERTEX_POINT ( 'NONE', #3022 ) ;
#445 = LINE ( 'NONE', #18307, #3466 ) ;
#446 = CARTESIAN_POINT ( 'NONE',  ( 43.34962307344081012, 54.89948385550240317, 2.184720259617164650 ) ) ;
#447 = CONICAL_SURFACE ( 'NONE', #7021, 8.105212085995399107, 1.221730476396037490 ) ;
#448 = ORIENTED_EDGE ( 'NONE', *, *, #5602, .F. ) ;
#449 = CARTESIAN_POINT ( 'NONE',  ( 1.171083334267915221, -24.65495046420793201, 9.999999999999998224 ) ) ;
#450 = ORIENTED_EDGE ( 'NONE', *, *, #569, .F. ) ;
#451 = CARTESIAN_POINT ( 'NONE',  ( 47.42335538002188144, 52.59948385550240602, 8.007379884777233059 ) ) ;
#452 = AXIS2_PLACEMENT_3D ( 'NONE', #12070, #1596, #13548 ) ;
#453 = DIRECTION ( 'NONE',  ( -1.000000000000000000, 0.000000000000000000, 0.000000000000000000 ) ) ;
#454 = CARTESIAN_POINT ( 'NONE',  ( 56.66441430157296821, 62.09948385550239891, 2.141517661632100111 ) ) ;
#455 = CARTESIAN_POINT ( 'NONE',  ( 4.071447262713887127, 2.020725942163686284, -3.499999999999999556 ) ) ;
#456 = CARTESIAN_POINT ( 'NONE',  ( 47.70284917648459100, 63.60051614449766078, 6.992620115222796251 ) ) ;
#457 = DIRECTION ( 'NONE',  ( 1.000000000000000000, 0.000000000000000000, 0.000000000000000000 ) ) ;
#458 = CARTESIAN_POINT ( 'NONE',  ( 49.97728705011488159, 57.49948385550241170, -7.000000000000000888 ) ) ;
#459 = CARTESIAN_POINT ( 'NONE',  ( 6.495567275915080430, -5.834887664329776236, 2.176274696337492837E-17 ) ) ;
#460 = ADVANCED_FACE ( 'NONE', ( #14594 ), #1653, .F. ) ;
#461 = ORIENTED_EDGE ( 'NONE', *, *, #12754, .F. ) ;
#462 = DIRECTION ( 'NONE',  ( 0.000000000000000000, 0.000000000000000000, 1.000000000000000000 ) ) ;
#463 = SHAPE_REPRESENTATION_RELATIONSHIP ( 'NONE' , 'NONE' ,  #10550, #17389 ) ;
#464 = VECTOR ( 'NONE', #12532, 1000.000000000000000 ) ;
#465 = EDGE_CURVE ( 'NONE', #17166, #14477, #13781, .T. ) ;
#466 = CARTESIAN_POINT ( 'NONE',  ( 54.13287192849676188, 52.29948385550240886, 5.649768623646098220 ) ) ;
#467 = PRESENTATION_STYLE_ASSIGNMENT (( #16854 ) ) ;
#468 = VERTEX_POINT ( 'NONE', #1547 ) ;
#469 = FACE_OUTER_BOUND ( 'NONE', #1033, .T. ) ;
#470 = VECTOR ( 'NONE', #5124, 1000.000000000000000 ) ;
#471 = ORIENTED_EDGE ( 'NONE', *, *, #4498, .F. ) ;
#472 = CARTESIAN_POINT ( 'NONE',  ( 42.63976443033212149, 64.00051614449765225, -0.02388180880514948964 ) ) ;
#473 = EDGE_LOOP ( 'NONE', ( #18813, #10177, #17658, #2063, #11824 ) ) ;
#474 = DIRECTION ( 'NONE',  ( 0.000000000000000000, -0.000000000000000000, 1.000000000000000000 ) ) ;
#475 = UNCERTAINTY_MEASURE_WITH_UNIT (LENGTH_MEASURE( 1.000000000000000082E-05 ), #13517, 'distance_accuracy_value', 'NONE');
#476 = CARTESIAN_POINT ( 'NONE',  ( 2.449293598294706513E-15, -20.00000000000000000, -50.00000000000000000 ) ) ;
#477 = CIRCLE ( 'NONE', #6723, 2.649999999999985700 ) ;
#478 = CARTESIAN_POINT ( 'NONE',  ( 55.71335778527780036, 58.90051614449766504, -1.832500667257213056 ) ) ;
#479 = DIRECTION ( 'NONE',  ( 0.9999419836444144449, 0.01077169184824096695, 0.000000000000000000 ) ) ;
#480 = CARTESIAN_POINT ( 'NONE',  ( 15.00000000000000178, -20.00000000000000000, -50.00000000000000000 ) ) ;
#481 = CARTESIAN_POINT ( 'NONE',  ( 6.534838248920899595, 5.903531555104835071, 8.098083288904839678E-18 ) ) ;
#482 = VECTOR ( 'NONE', #1590, 1000.000000000000000 ) ;
#483 = CARTESIAN_POINT ( 'NONE',  ( 52.57664461997821093, 57.40051614449767214, 8.007379884777206414 ) ) ;
#484 = ORIENTED_EDGE ( 'NONE', *, *, #4734, .T. ) ;
#485 = EDGE_LOOP ( 'NONE', ( #9928, #11888, #6922, #5916 ) ) ;
#486 = CARTESIAN_POINT ( 'NONE',  ( 0.04201760816083378175, -0.9730571234388133428, 4.999999999999997335 ) ) ;
#487 = SURFACE_SIDE_STYLE ('',( #18064 ) ) ;
#488 = VERTEX_POINT ( 'NONE', #18125 ) ;
#489 = DIRECTION ( 'NONE',  ( 1.000000000000000000, 0.000000000000000000, 0.000000000000000000 ) ) ;
#490 = PRODUCT_CONTEXT ( 'NONE', #11393, 'mechanical' ) ;
#491 = ORIENTED_EDGE ( 'NONE', *, *, #3042, .F. ) ;
#492 = CARTESIAN_POINT ( 'NONE',  ( 30.00000000000000000, -3.000000000000000000, 6.000000000000003553 ) ) ;
#493 = LINE ( 'NONE', #12738, #1897 ) ;
#494 = CIRCLE ( 'NONE', #15524, 1.000000000000000666 ) ;
#495 = CARTESIAN_POINT ( 'NONE',  ( 0.000000000000000000, 0.000000000000000000, -0.2800830152838844622 ) ) ;
#496 = UNCERTAINTY_MEASURE_WITH_UNIT (LENGTH_MEASURE( 1.000000000000000082E-05 ), #5087, 'distance_accuracy_value', 'NONE');
#497 = CARTESIAN_POINT ( 'NONE',  ( 45.60000000000000142, 0.000000000000000000, 0.000000000000000000 ) ) ;
#498 = CARTESIAN_POINT ( 'NONE',  ( 1.925929944387235853E-31, 15.00000000000001599, -9.000000000000000000 ) ) ;
#499 = CARTESIAN_POINT ( 'NONE',  ( -1.391697335622809950, -4.043246145443391448, -3.503898532754372575 ) ) ;
#500 = AXIS2_PLACEMENT_3D ( 'NONE', #15472, #12246, #13989 ) ;
#501 = CARTESIAN_POINT ( 'NONE',  ( 55.94051828345050836, 63.79948385550240886, -4.345558710429104465 ) ) ;
#502 = CARTESIAN_POINT ( 'NONE',  ( 3.806834918298644066, 1.084202172485504434E-15, 3.500000000000000000 ) ) ;
#503 = CARTESIAN_POINT ( 'NONE',  ( 42.38452918213188525, 63.09948385550240602, -2.450534656007040013 ) ) ;
#504 = EDGE_CURVE ( 'NONE', #8689, #19334, #374, .T. ) ;
#505 = CARTESIAN_POINT ( 'NONE',  ( 42.63976443033212860, 58.00051614449765225, -0.02388180880514948964 ) ) ;
#506 = DIRECTION ( 'NONE',  ( 1.000000000000000000, 0.000000000000000000, -0.000000000000000000 ) ) ;
#507 = CARTESIAN_POINT ( 'NONE',  ( -54.99999999999996447, -14.99999999999998579, 15.00000000000000178 ) ) ;
#508 = VERTEX_POINT ( 'NONE', #6242 ) ;
#509 = CARTESIAN_POINT ( 'NONE',  ( 4.197393957002303999, 7.772902908466098641E-14, -3.503767560748929810 ) ) ;
#510 = CARTESIAN_POINT ( 'NONE',  ( -0.2500000000000000000, -8.096141056083446585, 0.000000000000000000 ) ) ;
#511 = CARTESIAN_POINT ( 'NONE',  ( 45.86712807150323812, 63.29948385550240886, -5.649768623646098220 ) ) ;
#512 = ADVANCED_FACE ( 'NONE', ( #11928, #81 ), #6058, .F. ) ;
#513 = DIRECTION ( 'NONE',  ( 0.9781476007338055778, 0.2079116908177597867, 0.000000000000000000 ) ) ;
#514 = VERTEX_POINT ( 'NONE', #4873 ) ;
#515 = CARTESIAN_POINT ( 'NONE',  ( -54.99999999999996447, -6.999999999999985789, -10.00000000000000000 ) ) ;
#516 = AXIS2_PLACEMENT_3D ( 'NONE', #18287, #3472, #2000 ) ;
#517 = DIRECTION ( 'NONE',  ( -0.5000000000000019984, -0.8660254037844375974, 0.000000000000000000 ) ) ;
#518 = CARTESIAN_POINT ( 'NONE',  ( 51.97223112728254790, 62.39948385550240317, 5.992620115222778487 ) ) ;
#519 = DIRECTION ( 'NONE',  ( 1.000000000000000000, 0.000000000000000000, 0.000000000000000000 ) ) ;
#520 = CARTESIAN_POINT ( 'NONE',  ( -19.97007065299861850, -18.90625500492885180, -9.000000000000000000 ) ) ;
#521 = CARTESIAN_POINT ( 'NONE',  ( 41.58830220609386430, 62.00051614449766646, -0.02388180880514929535 ) ) ;
#522 = ADVANCED_FACE ( 'NONE', ( #10646 ), #7666, .F. ) ;
#523 = CARTESIAN_POINT ( 'NONE',  ( 44.88205777487401349, 61.80051614449766362, 3.688883143319584779 ) ) ;
#524 = CLOSED_SHELL ( 'NONE', ( #18637, #2934, #16284, #12275, #14309, #14146, #154, #5266, #18554, #3627, #6437, #13698, #10989, #17442, #12734, #18525, #12549, #4182, #11198, #4505, #11360, #6999, #9794, #15649, #16358, #2837, #940, #9380 ) ) ;
#525 = EDGE_CURVE ( 'NONE', #728, #14377, #18969, .T. ) ;
#526 = DIRECTION ( 'NONE',  ( -0.000000000000000000, -0.000000000000000000, 1.000000000000000000 ) ) ;
#527 = CARTESIAN_POINT ( 'NONE',  ( 6.390983399715594260, -5.837459000499769957, 0.1107755759658282380 ) ) ;
#528 = ORIENTED_EDGE ( 'NONE', *, *, #3643, .F. ) ;
#529 = AXIS2_PLACEMENT_3D ( 'NONE', #13472, #9051, #19389 ) ;
#530 = ORIENTED_EDGE ( 'NONE', *, *, #763, .F. ) ;
#531 = CARTESIAN_POINT ( 'NONE',  ( 20.00000000000000000, -14.99999999999999289, -20.00000000000000000 ) ) ;
#532 = VECTOR ( 'NONE', #14870, 1000.000000000000000 ) ;
#533 = ORIENTED_EDGE ( 'NONE', *, *, #13929, .T. ) ;
#534 = EDGE_CURVE ( 'NONE', #17889, #2561, #18649, .T. ) ;
#535 = CARTESIAN_POINT ( 'NONE',  ( -74.99999999999997158, 40.00000000000001421, -10.00000000000000000 ) ) ;
#536 = EDGE_CURVE ( 'NONE', #9835, #14591, #15254, .T. ) ;
#537 = ORIENTED_EDGE ( 'NONE', *, *, #13110, .T. ) ;
#538 = CARTESIAN_POINT ( 'NONE',  ( -14.17539641854921229, -5.891203581560112923, 9.000000000000000000 ) ) ;
#539 = CARTESIAN_POINT ( 'NONE',  ( 54.13287192849676188, 52.29948385550240886, 5.649768623646098220 ) ) ;
#540 = EDGE_CURVE ( 'NONE', #178, #11648, #7706, .T. ) ;
#541 = ORIENTED_EDGE ( 'NONE', *, *, #9614, .T. ) ;
#542 = CARTESIAN_POINT ( 'NONE',  ( -0.9996874511566050669, -39.97499999999999432, 9.000000000000000000 ) ) ;
#543 = ORIENTED_EDGE ( 'NONE', *, *, #13837, .F. ) ;
#544 = AXIS2_PLACEMENT_3D ( 'NONE', #1693, #7660, #14721 ) ;
#545 = CARTESIAN_POINT ( 'NONE',  ( 58.41169779390614281, 49.99948385550240459, -0.02388180880523160798 ) ) ;
#546 = CARTESIAN_POINT ( 'NONE',  ( 4.180232103119976728, 2.085387772176679366, -3.570466442734698820 ) ) ;
#547 = AXIS2_PLACEMENT_3D ( 'NONE', #18765, #4147, #14614 ) ;
#548 = CARTESIAN_POINT ( 'NONE',  ( 52.29715082351547295, 64.39948385550239607, 6.992620115222774047 ) ) ;
#549 = CARTESIAN_POINT ( 'NONE',  ( 4.175572532730929431, 2.061029303918044064, -3.569807470274393602 ) ) ;
#550 = DIRECTION ( 'NONE',  ( -0.000000000000000000, 0.000000000000000000, -1.000000000000000000 ) ) ;
#551 = AXIS2_PLACEMENT_3D ( 'NONE', #15450, #17327, #3884 ) ;
#552 = CARTESIAN_POINT ( 'NONE',  ( 44.05948171654945611, 60.20051614449764799, -4.345558710429044069 ) ) ;
#553 = CARTESIAN_POINT ( 'NONE',  ( -162.9999999999999716, -14.99999999999999645, 10.00000000000000000 ) ) ;
#554 = CARTESIAN_POINT ( 'NONE',  ( 50.02271294988512551, 60.49948385550240459, 7.000000000000000888 ) ) ;
#555 = CARTESIAN_POINT ( 'NONE',  ( -1.000000000000000000, -14.00000000000000000, 8.999999999999998224 ) ) ;
#556 = ORIENTED_EDGE ( 'NONE', *, *, #7640, .F. ) ;
#557 = VECTOR ( 'NONE', #8744, 1000.000000000000000 ) ;
#558 = ORIENTED_EDGE ( 'NONE', *, *, #7471, .T. ) ;
#559 = CARTESIAN_POINT ( 'NONE',  ( -72.99999999999997158, 1.000000000000000000, 6.000000000000000000 ) ) ;
#560 = AXIS2_PLACEMENT_3D ( 'NONE', #12362, #8144, #6676 ) ;
#561 = CARTESIAN_POINT ( 'NONE',  ( 56.65037692655918988, 51.89948385550241028, -2.184720259617163762 ) ) ;
#562 = DIRECTION ( 'NONE',  ( -1.000000000000000000, 0.000000000000000000, 0.000000000000000000 ) ) ;
#563 = ORIENTED_EDGE ( 'NONE', *, *, #9312, .F. ) ;
#564 = ORIENTED_EDGE ( 'NONE', *, *, #16830, .T. ) ;
#565 = CARTESIAN_POINT ( 'NONE',  ( 7.547063560035813063E-16, -3.202582148906732762, -1.452965002680431272 ) ) ;
#566 = ORIENTED_EDGE ( 'NONE', *, *, #5091, .F. ) ;
#567 = CARTESIAN_POINT ( 'NONE',  ( 17.79870116617236420, -10.87825472854593301, 9.000000000000000000 ) ) ;
#568 = ORIENTED_EDGE ( 'NONE', *, *, #6489, .F. ) ;
#569 = EDGE_CURVE ( 'NONE', #7216, #5656, #16454, .T. ) ;
#570 = CARTESIAN_POINT ( 'NONE',  ( 45.86712807150323812, 47.29948385550240886, -5.649768623646098220 ) ) ;
#571 = CARTESIAN_POINT ( 'NONE',  ( 18.68843350152500093, -27.12337372732038432, 0.000000000000000000 ) ) ;
#572 = CARTESIAN_POINT ( 'NONE',  ( 46.49166364869456913, 62.30051614449766362, -4.867452303228181343 ) ) ;
#573 = DIRECTION ( 'NONE',  ( -0.02045300604585054485, -0.9997908153927441699, -2.853726094247054863E-17 ) ) ;
#574=STYLED_ITEM('',(#19461),#14815);
#575 = EDGE_CURVE ( 'NONE', #17511, #6795, #14148, .T. ) ;
#576 = SURFACE_SIDE_STYLE ('',( #18545 ) ) ;
#577 = DIRECTION ( 'NONE',  ( -0.9999670257950099561, -0.008120795692649453515, 0.000000000000000000 ) ) ;
#578 = CARTESIAN_POINT ( 'NONE',  ( 52.57664461997821093, 61.40051614449765793, 8.007379884777206414 ) ) ;
#579 = MECHANICAL_DESIGN_GEOMETRIC_PRESENTATION_REPRESENTATION (  '', ( #14012 ), #4333 ) ;
#580 = ORIENTED_EDGE ( 'NONE', *, *, #7614, .F. ) ;
#581 = ORIENTED_EDGE ( 'NONE', *, *, #17054, .F. ) ;
#582 = DIRECTION ( 'NONE',  ( 1.000000000000000000, 0.000000000000000000, 0.000000000000000000 ) ) ;
#583 =( NAMED_UNIT ( * ) SI_UNIT ( $, .STERADIAN. ) SOLID_ANGLE_UNIT ( ) );
#584 = CARTESIAN_POINT ( 'NONE',  ( -31.74999999999995737, 0.000000000000000000, 0.000000000000000000 ) ) ;
#585 = VERTEX_POINT ( 'NONE', #10450 ) ;
#586 = CARTESIAN_POINT ( 'NONE',  ( -154.9999999999999716, -14.99999999999999645, 4.000000000000000000 ) ) ;
#587 = CIRCLE ( 'NONE', #6229, 5.999999999999977796 ) ;
#588 = CONICAL_SURFACE ( 'NONE', #5598, 5.000000000000000000, 1.047197551196600296 ) ;
#589 = CYLINDRICAL_SURFACE ( 'NONE', #2546, 5.000000000000000888 ) ;
#590 = VERTEX_POINT ( 'NONE', #18317 ) ;
#591 = EDGE_CURVE ( 'NONE', #11915, #8974, #13845, .T. ) ;
#592 = DIRECTION ( 'NONE',  ( -1.000000000000000000, 0.000000000000000000, 0.000000000000000000 ) ) ;
#593 = DIRECTION ( 'NONE',  ( -1.000000000000000000, -0.000000000000000000, -0.000000000000000000 ) ) ;
#594 = DIRECTION ( 'NONE',  ( -0.000000000000000000, -0.000000000000000000, -1.000000000000000000 ) ) ;
#595 = LINE ( 'NONE', #15210, #9936 ) ;
#596 = CARTESIAN_POINT ( 'NONE',  ( 55.08986747509847248, 45.79948385550240886, -3.727524721679197572 ) ) ;
#597 = CARTESIAN_POINT ( 'NONE',  ( -10.93224627749309796, -3.252283996668733135, 0.000000000000000000 ) ) ;
#598 = CARTESIAN_POINT ( 'NONE',  ( 41.58830220609386430, 58.99948385550239749, 0.02388180880523263147 ) ) ;
#599 = VECTOR ( 'NONE', #11017, 1000.000000000000000 ) ;
#600 = CARTESIAN_POINT ( 'NONE',  ( 47.74827507625469281, 62.40051614449766504, -7.007379884777203749 ) ) ;
#601 = VECTOR ( 'NONE', #10729, 1000.000000000000000 ) ;
#602 = B_SPLINE_CURVE_WITH_KNOTS ( 'NONE', 3,
 ( #12165, #19041, #11456, #9987, #5485, #17465 ),
 .UNSPECIFIED., .F., .F.,
 ( 4, 2, 4 ),
 ( 0.01103795672827925789, 0.01206113196748797960, 0.01308430720669670130 ),
 .UNSPECIFIED. ) ;
#603 = LINE ( 'NONE', #2181, #4937 ) ;
#604 = CARTESIAN_POINT ( 'NONE',  ( 2.000000000000000000, 1.773042676681340524, -2.059984127722458425E-15 ) ) ;
#605 = MECHANICAL_DESIGN_GEOMETRIC_PRESENTATION_REPRESENTATION (  '', ( #15624 ), #12814 ) ;
#606 = VERTEX_POINT ( 'NONE', #12312 ) ;
#607 = CYLINDRICAL_SURFACE ( 'NONE', #15492, 15.00000000000000000 ) ;
#608 = CARTESIAN_POINT ( 'NONE',  ( -54.99999999999996447, -14.99999999999998579, 15.00000000000000000 ) ) ;
#609 = CARTESIAN_POINT ( 'NONE',  ( 42.63976443033212149, 48.00051614449766646, -0.02388180880514948964 ) ) ;
#610 = VECTOR ( 'NONE', #15203, 1000.000000000000000 ) ;
#611 = DIRECTION ( 'NONE',  ( 1.000000000000000000, 0.000000000000000000, 0.000000000000000000 ) ) ;
#612 = DIRECTION ( 'NONE',  ( -1.000000000000000000, 0.000000000000000000, 0.000000000000000000 ) ) ;
#613 = ORIENTED_EDGE ( 'NONE', *, *, #8437, .T. ) ;
#614 = CARTESIAN_POINT ( 'NONE',  ( 2.449293598294706513E-15, -20.00000000000000000, 15.00000000000000355 ) ) ;
#615 = LINE ( 'NONE', #12469, #11701 ) ;
#616 = CARTESIAN_POINT ( 'NONE',  ( 43.69122665457040000, 60.99948385550241170, 0.02388180880521036456 ) ) ;
#617 = DIRECTION ( 'NONE',  ( -0.000000000000000000, -0.000000000000000000, -1.000000000000000000 ) ) ;
#618 = CARTESIAN_POINT ( 'NONE',  ( 54.09612160359786515, 47.69948385550240744, -5.676469297603166098 ) ) ;
#619 = AXIS2_PLACEMENT_3D ( 'NONE', #15609, #14025, #15907 ) ;
#620 = CARTESIAN_POINT ( 'NONE',  ( -11.75570504584948139, -3.819660112501066518, -9.000000000000000000 ) ) ;
#621 = CARTESIAN_POINT ( 'NONE',  ( 56.81924384183006538, 56.80051614449764941, -4.924951120819380357 ) ) ;
#622 = CARTESIAN_POINT ( 'NONE',  ( 44.88205777487401349, 59.80051614449766362, 3.688883143319584779 ) ) ;
#623 = CYLINDRICAL_SURFACE ( 'NONE', #10678, 2.649999999999988365 ) ;
#624 = CARTESIAN_POINT ( 'NONE',  ( 6.541334219041339715, -5.921300567812618709, 0.03049376373817737351 ) ) ;
#625 = CIRCLE ( 'NONE', #12841, 20.00000000000000000 ) ;
#626 = ORIENTED_EDGE ( 'NONE', *, *, #1141, .T. ) ;
#627 = CIRCLE ( 'NONE', #7209, 0.5999999999999998668 ) ;
#628 = VERTEX_POINT ( 'NONE', #2031 ) ;
#629 = PLANE ( 'NONE',  #12484 ) ;
#630 = ORIENTED_EDGE ( 'NONE', *, *, #16372, .F. ) ;
#631 = CARTESIAN_POINT ( 'NONE',  ( 3.948095570617042860, 0.6965071952218068185, 3.500000000000155875 ) ) ;
#632 = CIRCLE ( 'NONE', #5645, 1.000000000000000000 ) ;
#633 = ORIENTED_EDGE ( 'NONE', *, *, #4119, .T. ) ;
#634 = FACE_OUTER_BOUND ( 'NONE', #11741, .T. ) ;
#635 = EDGE_CURVE ( 'NONE', #6724, #14776, #17314, .T. ) ;
#636 = CARTESIAN_POINT ( 'NONE',  ( 57.36023556966787851, 53.99948385550239749, -0.02388180880522424582 ) ) ;
#637 = EDGE_LOOP ( 'NONE', ( #3972, #2, #1409, #7912 ) ) ;
#638 = CARTESIAN_POINT ( 'NONE',  ( 6.466260427357664042, -2.904280683598015500, -5.030361703432624232 ) ) ;
#639 = EDGE_LOOP ( 'NONE', ( #2645, #1504, #14829, #11525 ) ) ;
#640 =( REPRESENTATION_RELATIONSHIP ('NONE','NONE', #16703, #19357 ) REPRESENTATION_RELATIONSHIP_WITH_TRANSFORMATION ( #7650 )SHAPE_REPRESENTATION_RELATIONSHIP( ) );
#641 = CARTESIAN_POINT ( 'NONE',  ( 56.79116909180255135, 49.79948385550240175, -4.963592699179005585 ) ) ;
#642 = CIRCLE ( 'NONE', #6581, 9.999999999999998224 ) ;
#643 = FACE_OUTER_BOUND ( 'NONE', #735, .T. ) ;
#644 = EDGE_CURVE ( 'NONE', #9042, #12835, #16688, .T. ) ;
#645 = CARTESIAN_POINT ( 'NONE',  ( 44.88205777487398507, 47.19948385550240744, -3.688883143319540814 ) ) ;
#646 = CARTESIAN_POINT ( 'NONE',  ( 4.132952817037867987, 2.031684012687259511, -3.518979934899751694 ) ) ;
#647 = CARTESIAN_POINT ( 'NONE',  ( -4.747884751462026820, -5.143694235355983579, -0.8000000000000000444 ) ) ;
#648 = AXIS2_PLACEMENT_3D ( 'NONE', #17257, #13019, #13119 ) ;
#649 = CIRCLE ( 'NONE', #7227, 5.000000000000007994 ) ;
#650 = CARTESIAN_POINT ( 'NONE',  ( 43.33558569842706021, 57.90051614449766504, 2.141517661632167169 ) ) ;
#651 = EDGE_CURVE ( 'NONE', #13093, #10178, #4152, .T. ) ;
#652 = ADVANCED_FACE ( 'NONE', ( #12498 ), #3409, .F. ) ;
#653 = AXIS2_PLACEMENT_3D ( 'NONE', #11372, #801, #895 ) ;
#654 = CARTESIAN_POINT ( 'NONE',  ( 57.36023556966787851, 55.99948385550239038, -0.02388180880522424582 ) ) ;
#655 = CARTESIAN_POINT ( 'NONE',  ( 6.367873360227559232, -5.773502691896263528, 0.000000000000000000 ) ) ;
#656 = CARTESIAN_POINT ( 'NONE',  ( 6.245824673232967861, -4.939548505213401164, 1.655093584844986143 ) ) ;
#657 = ORIENTED_EDGE ( 'NONE', *, *, #347, .T. ) ;
#658 = ADVANCED_FACE ( 'NONE', ( #13962 ), #8085, .T. ) ;
#659 = SHAPE_REPRESENTATION ( 'idle-roller mover', ( #10359 ), #7771 ) ;
#660 = VERTEX_POINT ( 'NONE', #9650 ) ;
#661 = CARTESIAN_POINT ( 'NONE',  ( -9.037824375505556063, -2.158539001597498341, 9.000000000000000000 ) ) ;
#662 = AXIS2_PLACEMENT_3D ( 'NONE', #14086, #13891, #15467 ) ;
#663 = CARTESIAN_POINT ( 'NONE',  ( 56.65037692655918988, 53.89948385550240317, -2.184720259617163762 ) ) ;
#664 = CARTESIAN_POINT ( 'NONE',  ( 1.267864665261691752E-11, -20.00000000000000000, 9.999999999999998224 ) ) ;
#665 = CIRCLE ( 'NONE', #9128, 0.1000000000000011297 ) ;
#666 = VERTEX_POINT ( 'NONE', #11028 ) ;
#667 = ORIENTED_EDGE ( 'NONE', *, *, #12974, .T. ) ;
#668 = DIRECTION ( 'NONE',  ( -0.6691306063588624564, 0.7431448254773903583, 0.000000000000000000 ) ) ;
#669 = EDGE_CURVE ( 'NONE', #11235, #2243, #10628, .T. ) ;
#670 = EDGE_CURVE ( 'NONE', #10950, #14856, #10929, .T. ) ;
#671 = VERTEX_POINT ( 'NONE', #6520 ) ;
#672 = CARTESIAN_POINT ( 'NONE',  ( 43.34962307344078880, 64.10051614449766078, -2.184720259617096705 ) ) ;
#673 = ORIENTED_EDGE ( 'NONE', *, *, #4548, .F. ) ;
#674 = FACE_OUTER_BOUND ( 'NONE', #12815, .T. ) ;
#675 = CARTESIAN_POINT ( 'NONE',  ( -2.852594293689151105E-15, 3.375361811986501426, -1.153701847711632311 ) ) ;
#676 = CARTESIAN_POINT ( 'NONE',  ( 46.45491332379576477, 61.70051614449766220, 4.840751629271188961 ) ) ;
#677 = CARTESIAN_POINT ( 'NONE',  ( -18.89043790736547379, -17.90943073464699609, -9.000000000000000000 ) ) ;
#678 = LINE ( 'NONE', #3432, #2073 ) ;
#679 = LINE ( 'NONE', #298, #24 ) ;
#680 = CIRCLE ( 'NONE', #11624, 12.49999999999999645 ) ;
#681 = VECTOR ( 'NONE', #14209, 1000.000000000000000 ) ;
#682 = CARTESIAN_POINT ( 'NONE',  ( 49.97728705011495265, 59.50051614449765935, 8.000000000000001776 ) ) ;
#683 = PRODUCT ( 'circlip for shafts normal_din_Circlip DIN 471 - 10 x 1', 'circlip for shafts normal_din_Circlip DIN 471 - 10 x 1', '', ( #1686 ) ) ;
#684 = ORIENTED_EDGE ( 'NONE', *, *, #1869, .T. ) ;
#685 = ORIENTED_EDGE ( 'NONE', *, *, #11171, .T. ) ;
#686 = FACE_OUTER_BOUND ( 'NONE', #12366, .T. ) ;
#687 = DIRECTION ( 'NONE',  ( -1.000000000000000000, -0.000000000000000000, -0.000000000000000000 ) ) ;
#688 = ITEM_DEFINED_TRANSFORMATION ( 'NONE', 'NONE', #3241,  #10359 ) ;
#689 = ORIENTED_EDGE ( 'NONE', *, *, #14219, .T. ) ;
#690 = CARTESIAN_POINT ( 'NONE',  ( -29.99999999999999645, 40.00000000000000000, -9.999999999999998224 ) ) ;
#691 = B_SPLINE_CURVE_WITH_KNOTS ( 'NONE', 3,
 ( #18613, #5537, #5153, #3691, #8492, #11127, #2238, #17423, #17230, #15944, #18906, #8283, #8196, #11223, #14467, #18805 ),
 .UNSPECIFIED., .F., .F.,
 ( 4, 3, 3, 3, 3, 4 ),
 ( 0.000000000000000000, 5.303647860849932744E-05, 0.0001057093501027352823, 0.0001642058037231763413, 0.0002210073443958810151, 0.0002236769549542870245 ),
 .UNSPECIFIED. ) ;
#692 = CARTESIAN_POINT ( 'NONE',  ( 0.000000000000000000, 6.123233995736766282E-16, -5.000000000000000000 ) ) ;
#693 = ORIENTED_EDGE ( 'NONE', *, *, #17667, .F. ) ;
#694 = LINE ( 'NONE', #6666, #10977 ) ;
#695 = DIRECTION ( 'NONE',  ( 1.000000000000000000, 0.000000000000000000, 0.000000000000000000 ) ) ;
#696 = VECTOR ( 'NONE', #16652, 1000.000000000000000 ) ;
#697 = CARTESIAN_POINT ( 'NONE',  ( -1.249999999999997558, 0.000000000000000000, 0.000000000000000000 ) ) ;
#698 = FACE_BOUND ( 'NONE', #76, .T. ) ;
#699 = PLANE ( 'NONE',  #16848 ) ;
#700 = CARTESIAN_POINT ( 'NONE',  ( 46.49166364869460466, 46.69948385550240744, 4.867452303228209765 ) ) ;
#701 = DIRECTION ( 'NONE',  ( -1.000000000000000000, -1.387778780781445676E-16, 0.000000000000000000 ) ) ;
#702 = CARTESIAN_POINT ( 'NONE',  ( 42.39856655714566358, 60.89948385550241028, 2.493737253992119207 ) ) ;
#703 = CARTESIAN_POINT ( 'NONE',  ( 45.86712807150329496, 63.70051614449766220, 5.649768623646139964 ) ) ;
#704 = CIRCLE ( 'NONE', #1338, 5.000000000000000888 ) ;
#705 = DIRECTION ( 'NONE',  ( 0.000000000000000000, 0.000000000000000000, -1.000000000000000000 ) ) ;
#706 =( NAMED_UNIT ( * ) PLANE_ANGLE_UNIT ( ) SI_UNIT ( $, .RADIAN. ) );
#707 = ADVANCED_FACE ( 'NONE', ( #9553 ), #15544, .F. ) ;
#708 = CARTESIAN_POINT ( 'NONE',  ( 0.000000000000000000, 0.000000000000000000, 0.000000000000000000 ) ) ;
#709 = ORIENTED_EDGE ( 'NONE', *, *, #9739, .T. ) ;
#710 = EDGE_CURVE ( 'NONE', #5344, #15631, #17127, .T. ) ;
#711 = CYLINDRICAL_SURFACE ( 'NONE', #16596, 12.49999999999999645 ) ;
#712 = CARTESIAN_POINT ( 'NONE',  ( 44.03140696652198471, 53.80051614449766362, 4.306917132069485454 ) ) ;
#713 = CARTESIAN_POINT ( 'NONE',  ( 4.124214193018075569, -2.028338413290941666, 3.513185186763556622 ) ) ;
#714 = LINE ( 'NONE', #15224, #7109 ) ;
#715 = EDGE_LOOP ( 'NONE', ( #8908, #4460, #558, #11992 ) ) ;
#716 = CARTESIAN_POINT ( 'NONE',  ( -4.158233816355060064, -39.56295201467614220, 9.000000000000000000 ) ) ;
#717 = LINE ( 'NONE', #6688, #13278 ) ;
#718 = DIRECTION ( 'NONE',  ( -1.000000000000000000, 0.000000000000000000, 0.000000000000000000 ) ) ;
#719 =( NAMED_UNIT ( * ) SI_UNIT ( $, .STERADIAN. ) SOLID_ANGLE_UNIT ( ) );
#720 = AXIS2_PLACEMENT_3D ( 'NONE', #7066, #13048, #19057 ) ;
#721 = CARTESIAN_POINT ( 'NONE',  ( 17.32050807568887052, -29.99999999999984013, 9.000000000000000000 ) ) ;
#722 = CARTESIAN_POINT ( 'NONE',  ( 47.42335538002180328, 58.40051614449765793, -8.007379884777206414 ) ) ;
#723 = CARTESIAN_POINT ( 'NONE',  ( 44.30067958973594955, 62.10051614449765367, -1.875703265242155693 ) ) ;
#724 = FACE_OUTER_BOUND ( 'NONE', #3141, .T. ) ;
#725 = CYLINDRICAL_SURFACE ( 'NONE', #9088, 1.999999999999998224 ) ;
#726 = ORIENTED_EDGE ( 'NONE', *, *, #14827, .T. ) ;
#727 = ORIENTED_EDGE ( 'NONE', *, *, #14442, .F. ) ;
#728 = VERTEX_POINT ( 'NONE', #17418 ) ;
#729 = PLANE ( 'NONE',  #15634 ) ;
#730 = VERTEX_POINT ( 'NONE', #1229 ) ;
#731 = CARTESIAN_POINT ( 'NONE',  ( 0.9999999999999997780, -6.008326913195983998, 0.000000000000000000 ) ) ;
#732 = ORIENTED_EDGE ( 'NONE', *, *, #14030, .F. ) ;
#733 = CARTESIAN_POINT ( 'NONE',  ( 2.899426713160750069, -23.82535289025860337, -8.999999999999996447 ) ) ;
#734 = CARTESIAN_POINT ( 'NONE',  ( 43.34962307344081012, 60.89948385550241028, 2.184720259617164650 ) ) ;
#735 = EDGE_LOOP ( 'NONE', ( #6903, #13575, #566 ) ) ;
#736 = DIRECTION ( 'NONE',  ( -1.000000000000000000, 0.000000000000000000, -0.000000000000000000 ) ) ;
#737 = VERTEX_POINT ( 'NONE', #15940 ) ;
#738 = CARTESIAN_POINT ( 'NONE',  ( 47.42335538002188144, 54.59948385550240602, 8.007379884777233059 ) ) ;
#739 = FACE_OUTER_BOUND ( 'NONE', #15662, .T. ) ;
#740 = CARTESIAN_POINT ( 'NONE',  ( 44.03140696652192787, 65.19948385550240744, -4.306917132069425058 ) ) ;
#741 = DIRECTION ( 'NONE',  ( 0.000000000000000000, 1.000000000000000000, 0.000000000000000000 ) ) ;
#742 = CARTESIAN_POINT ( 'NONE',  ( -0.1085714285714285687, -3.798448662927795372, -0.8000000000000000444 ) ) ;
#743 = CARTESIAN_POINT ( 'NONE',  ( 56.65037692655921120, 61.10051614449766078, 2.184720259617097593 ) ) ;
#744 = CARTESIAN_POINT ( 'NONE',  ( 44.28664221472220675, 65.09948385550239891, -1.832500667257165317 ) ) ;
#745 = CARTESIAN_POINT ( 'NONE',  ( 43.34962307344081012, 58.89948385550241028, 2.184720259617164650 ) ) ;
#746 = CARTESIAN_POINT ( 'NONE',  ( -4.000000000000000000, -2.309401076758512694, -3.433295621305382461 ) ) ;
#747 = CARTESIAN_POINT ( 'NONE',  ( 2.449293598294706513E-15, -20.00000000000000000, -9.000000000000000000 ) ) ;
#748 = EDGE_CURVE ( 'NONE', #6937, #6699, #5739, .T. ) ;
#749 = ORIENTED_EDGE ( 'NONE', *, *, #15883, .T. ) ;
#750 = ORIENTED_EDGE ( 'NONE', *, *, #344, .F. ) ;
#751 = DIRECTION ( 'NONE',  ( 0.000000000000000000, 0.000000000000000000, -1.000000000000000000 ) ) ;
#752 = EDGE_CURVE ( 'NONE', #928, #17028, #8377, .T. ) ;
#753 = CIRCLE ( 'NONE', #14189, 20.00000000000000000 ) ;
#754 = CARTESIAN_POINT ( 'NONE',  ( 45.90387839640214196, 58.69948385550240033, 5.676469297603166098 ) ) ;
#755 = CARTESIAN_POINT ( 'NONE',  ( 4.050880675075949178, 1.379097446046194220, 3.567934390854430760 ) ) ;
#756 = ORIENTED_EDGE ( 'NONE', *, *, #9160, .F. ) ;
#757 = ORIENTED_EDGE ( 'NONE', *, *, #3293, .T. ) ;
#758 = CIRCLE ( 'NONE', #18298, 0.4999999999999978351 ) ;
#759 = DIRECTION ( 'NONE',  ( 0.3420201433256622736, 1.150791560227853228E-16, 0.9396926207859106484 ) ) ;
#760 = EDGE_LOOP ( 'NONE', ( #5028, #7175, #2540, #12004 ) ) ;
#761 = CARTESIAN_POINT ( 'NONE',  ( 19.76107906696387317, -16.91783288752825243, -9.000000000000000000 ) ) ;
#762 = VERTEX_POINT ( 'NONE', #17709 ) ;
#763 = EDGE_CURVE ( 'NONE', #10243, #10468, #4266, .T. ) ;
#764 = CARTESIAN_POINT ( 'NONE',  ( 55.96859303347804371, 46.19948385550238612, 4.306917132069425946 ) ) ;
#765 = CARTESIAN_POINT ( 'NONE',  ( -4.999999999999998224, -20.00000000000000000, -8.999999999999998224 ) ) ;
#766 = EDGE_CURVE ( 'NONE', #17828, #5258, #15091, .T. ) ;
#767 = CARTESIAN_POINT ( 'NONE',  ( 53.54508667620424234, 58.70051614449765509, -4.840751629271188961 ) ) ;
#768 = CARTESIAN_POINT ( 'NONE',  ( 10.00000000000000000, 0.000000000000000000, 9.999999999999998224 ) ) ;
#769 = DIRECTION ( 'NONE',  ( -0.000000000000000000, 0.8660254037844392627, 0.4999999999999990008 ) ) ;
#770 = DIRECTION ( 'NONE',  ( -0.000000000000000000, -0.000000000000000000, 1.000000000000000000 ) ) ;
#771 = AXIS2_PLACEMENT_3D ( 'NONE', #7468, #11769, #12166 ) ;
#772 = EDGE_CURVE ( 'NONE', #6867, #16920, #13086, .T. ) ;
#773 = EDGE_CURVE ( 'NONE', #14662, #8385, #13542, .T. ) ;
#774 = ORIENTED_EDGE ( 'NONE', *, *, #6694, .T. ) ;
#775 = ORIENTED_EDGE ( 'NONE', *, *, #19061, .T. ) ;
#776 = DIRECTION ( 'NONE',  ( -1.000000000000000000, 0.000000000000000000, 0.000000000000000000 ) ) ;
#777 = SURFACE_STYLE_FILL_AREA ( #6555 ) ;
#778 = DIRECTION ( 'NONE',  ( 0.9999419836444144449, 0.01077169184824096695, 0.000000000000000000 ) ) ;
#779 = CONTEXT_DEPENDENT_SHAPE_REPRESENTATION ( #6653, #14610 ) ;
#780 = ADVANCED_BREP_SHAPE_REPRESENTATION ( '', ( #2030, #10359 ), #6832 ) ;
#781 = ORIENTED_EDGE ( 'NONE', *, *, #10591, .F. ) ;
#782 = CARTESIAN_POINT ( 'NONE',  ( 6.271006797790669829, -0.9853839345309097775, -5.106080050406711202 ) ) ;
#783 = EDGE_CURVE ( 'NONE', #14027, #16215, #3977, .T. ) ;
#784 = CARTESIAN_POINT ( 'NONE',  ( -52.34999999999998010, -14.99999999999998579, 10.00000000000000000 ) ) ;
#785 = CIRCLE ( 'NONE', #2368, 4.599999999999999645 ) ;
#787 = EDGE_CURVE ( 'NONE', #6069, #5525, #6343, .T. ) ;
#786 = ORIENTED_EDGE ( 'NONE', *, *, #16950, .T. ) ;
#788 = AXIS2_PLACEMENT_3D ( 'NONE', #11144, #17151, #5374 ) ;
#789 = ADVANCED_FACE ( 'NONE', ( #5437, #16232 ), #11611, .T. ) ;
#790 = DIRECTION ( 'NONE',  ( 1.000000000000000000, 0.000000000000000000, 0.000000000000000000 ) ) ;
#791 = CARTESIAN_POINT ( 'NONE',  ( -11.75570504584948139, -3.819660112501066518, -9.000000000000000000 ) ) ;
#792 = CARTESIAN_POINT ( 'NONE',  ( 4.175572532730932096, 4.122058607836116551, 1.170198429493232648E-15 ) ) ;
#793 = LINE ( 'NONE', #14596, #4213 ) ;
#794 = CIRCLE ( 'NONE', #14566, 7.000000000000000000 ) ;
#795 = CARTESIAN_POINT ( 'NONE',  ( -2.100000000000000089, 2.571758278209441957E-16, -0.2800830152838844622 ) ) ;
#796 = CARTESIAN_POINT ( 'NONE',  ( 54.13287192849676188, 64.29948385550241596, 5.649768623646098220 ) ) ;
#797 = DIRECTION ( 'NONE',  ( 0.000000000000000000, -0.000000000000000000, 1.000000000000000000 ) ) ;
#798 = CARTESIAN_POINT ( 'NONE',  ( 57.60143344285433642, 63.89948385550240317, -2.493737253992118319 ) ) ;
#799 = CARTESIAN_POINT ( 'NONE',  ( 52.29715082351538769, 62.60051614449766078, -6.992620115222796251 ) ) ;
#800 = LINE ( 'NONE', #6771, #1505 ) ;
#801 = DIRECTION ( 'NONE',  ( 0.9914448613738102711, -0.1305261922200524338, 0.000000000000000000 ) ) ;
#802 = DIRECTION ( 'NONE',  ( 0.000000000000000000, -1.000000000000000000, 0.000000000000000000 ) ) ;
#803 = EDGE_LOOP ( 'NONE', ( #2536, #10777, #7323, #12200 ) ) ;
#804 = VECTOR ( 'NONE', #311, 1000.000000000000000 ) ;
#805 = LINE ( 'NONE', #17384, #2831 ) ;
#806 = CARTESIAN_POINT ( 'NONE',  ( 55.94051828345054389, 55.20051614449766220, 4.345558710429044957 ) ) ;
#807 = CARTESIAN_POINT ( 'NONE',  ( 4.142654963991859063, -2.035398498734348305, 3.525413613457315076 ) ) ;
#808 =( GEOMETRIC_REPRESENTATION_CONTEXT ( 3 ) GLOBAL_UNCERTAINTY_ASSIGNED_CONTEXT ( ( #5003 ) ) GLOBAL_UNIT_ASSIGNED_CONTEXT ( ( #1553, #2931, #11933 ) ) REPRESENTATION_CONTEXT ( 'NONE', 'WORKASPACE' ) );
#809 = DIRECTION ( 'NONE',  ( 0.000000000000000000, 0.000000000000000000, -1.000000000000000000 ) ) ;
#810 = CARTESIAN_POINT ( 'NONE',  ( -74.99999999999997158, -3.000000000000000000, -20.00000000000000000 ) ) ;
#811 = CARTESIAN_POINT ( 'NONE',  ( 3.175194142251959395, -0.2536549670829222891, 0.000000000000000000 ) ) ;
#812 = DIRECTION ( 'NONE',  ( -1.000000000000000000, 0.000000000000000000, 0.000000000000000000 ) ) ;
#813 = EDGE_CURVE ( 'NONE', #7075, #6422, #11344, .T. ) ;
#814 = DIRECTION ( 'NONE',  ( -1.000000000000000000, -0.000000000000000000, -0.000000000000000000 ) ) ;
#815 = CARTESIAN_POINT ( 'NONE',  ( 47.74827507625478518, 48.59948385550239180, 7.007379884777227730 ) ) ;
#816 = LINE ( 'NONE', #6596, #2010 ) ;
#817 = CARTESIAN_POINT ( 'NONE',  ( 49.97728705011486738, 47.49948385550240459, -8.000000000000001776 ) ) ;
#818 = CIRCLE ( 'NONE', #16168, 5.400000000000000355 ) ;
#819 = EDGE_CURVE ( 'NONE', #6895, #18142, #941, .T. ) ;
#820 = CARTESIAN_POINT ( 'NONE',  ( 55.69932041026405045, 61.10051614449766788, 1.875703265242156359 ) ) ;
#821 = CARTESIAN_POINT ( 'NONE',  ( 2.141980652367355464, -6.189445006155633422, -0.8000000000000000444 ) ) ;
#822 = CARTESIAN_POINT ( 'NONE',  ( 6.390983631292896483, 3.014665224428355383, 4.999999999999999112 ) ) ;
#823 = ORIENTED_EDGE ( 'NONE', *, *, #2475, .T. ) ;
#824 = AXIS2_PLACEMENT_3D ( 'NONE', #3051, #9010, #1576 ) ;
#825 = ORIENTED_EDGE ( 'NONE', *, *, #1368, .F. ) ;
#826 = EDGE_LOOP ( 'NONE', ( #10240, #13120, #5556, #14929, #17534, #17311, #15195, #957, #13396, #3693, #849, #8118, #17435, #10866, #18404, #3444, #17944, #1819, #10052, #1799, #14812, #13494, #6030, #667, #4210, #4378, #19128, #14482, #9173, #14661, #18119, #5853, #10615, #17650, #8610, #6461, #354, #8873, #329, #14105, #1118, #11724, #12303, #13901, #12807, #3007, #1875, #3118, #11250, #3617, #6139, #1702, #5470, #3801, #428, #9248, #2440, #8586, #4995, #5364, #10159, #6076, #14755, #11333, #9586, #2359, #9658, #10533, #5646, #225, #18731, #17801, #14491, #16083, #10253 ) ) ;
#827 = CARTESIAN_POINT ( 'NONE',  ( -0.9996874511566102850, -0.02500000000000036915, 0.000000000000000000 ) ) ;
#828 = VERTEX_POINT ( 'NONE', #19294 ) ;
#829 = CARTESIAN_POINT ( 'NONE',  ( -32.00000000000000000, 3.000000000000000000, 5.999999999999998224 ) ) ;
#830 = EDGE_LOOP ( 'NONE', ( #4840, #13776, #3319, #7867, #626, #1665 ) ) ;
#831 = CARTESIAN_POINT ( 'NONE',  ( -1.250000000000001110, 0.000000000000000000, 0.000000000000000000 ) ) ;
#832 = CARTESIAN_POINT ( 'NONE',  ( 56.65037692655918988, 57.89948385550240317, -2.184720259617163762 ) ) ;
#833 = ORIENTED_EDGE ( 'NONE', *, *, #15508, .T. ) ;
#834 = CARTESIAN_POINT ( 'NONE',  ( 0.3108895250736384841, -2.416698868092693075, -5.000000000000000000 ) ) ;
#835 = ORIENTED_EDGE ( 'NONE', *, *, #16599, .T. ) ;
#836 = CARTESIAN_POINT ( 'NONE',  ( 45.27934281921075410, 55.29948385550240175, -6.458785618021043895 ) ) ;
#837 = CARTESIAN_POINT ( 'NONE',  ( 4.086262841041386373, 2.102637316508698451, -3.499999999999999556 ) ) ;
#838 = CARTESIAN_POINT ( 'NONE',  ( 51.92680522751233951, 51.59948385550240602, -6.007379884777223289 ) ) ;
#839 = DIRECTION ( 'NONE',  ( 0.000000000000000000, -0.000000000000000000, 1.000000000000000000 ) ) ;
#840 = DIRECTION ( 'NONE',  ( 0.5000000000000013323, -0.8660254037844379305, 0.000000000000000000 ) ) ;
#841 = CARTESIAN_POINT ( 'NONE',  ( 44.03140696652198471, 61.80051614449767072, 4.306917132069485454 ) ) ;
#842 = CARTESIAN_POINT ( 'NONE',  ( 49.97728705011488870, 65.49948385550240459, -6.000000000000000888 ) ) ;
#843 = CIRCLE ( 'NONE', #5244, 4.000000000000000000 ) ;
#844 = CARTESIAN_POINT ( 'NONE',  ( 56.66441430157296821, 60.09948385550240602, 2.141517661632100111 ) ) ;
#845 = CARTESIAN_POINT ( 'NONE',  ( -54.99999999999996447, -6.999999999999985789, 15.00000000000000000 ) ) ;
#846 = AXIS2_PLACEMENT_3D ( 'NONE', #4289, #19020, #14574 ) ;
#847 = LINE ( 'NONE', #6820, #14709 ) ;
#848 = VERTEX_POINT ( 'NONE', #18900 ) ;
#849 = ORIENTED_EDGE ( 'NONE', *, *, #8720, .T. ) ;
#850 = FACE_OUTER_BOUND ( 'NONE', #6828, .T. ) ;
#851 = ORIENTED_EDGE ( 'NONE', *, *, #8320, .T. ) ;
#852 = CARTESIAN_POINT ( 'NONE',  ( 43.33558569842703179, 61.09948385550240602, -2.141517661632099223 ) ) ;
#853 = CARTESIAN_POINT ( 'NONE',  ( 0.000000000000000000, 0.000000000000000000, -1.000000000000000000 ) ) ;
#854 = EDGE_LOOP ( 'NONE', ( #10763, #14737 ) ) ;
#855 = ORIENTED_EDGE ( 'NONE', *, *, #534, .T. ) ;
#856 = CARTESIAN_POINT ( 'NONE',  ( -154.8505191518487152, -18.79705879280739467, -15.00000000000000000 ) ) ;
#857 = ORIENTED_EDGE ( 'NONE', *, *, #18164, .T. ) ;
#858 = DIRECTION ( 'NONE',  ( -0.9781476007338035794, -0.2079116908177690293, 0.000000000000000000 ) ) ;
#859 = EDGE_LOOP ( 'NONE', ( #17158, #4161, #12348, #6970 ) ) ;
#860 = CIRCLE ( 'NONE', #5248, 2.447112362156698140 ) ;
#861 = DIRECTION ( 'NONE',  ( -1.000000000000000000, 0.000000000000000000, 0.000000000000000000 ) ) ;
#862 = CARTESIAN_POINT ( 'NONE',  ( -74.99999999999997158, -1.000000000000000000, 6.000000000000001776 ) ) ;
#863 = CARTESIAN_POINT ( 'NONE',  ( 46.45491332379576477, 59.70051614449766220, 4.840751629271188961 ) ) ;
#864 = CYLINDRICAL_SURFACE ( 'NONE', #15186, 20.00000000000000000 ) ;
#865 = CARTESIAN_POINT ( 'NONE',  ( 2.449293598294706513E-15, -20.00000000000000000, -9.000000000000000000 ) ) ;
#866 = DIRECTION ( 'NONE',  ( 1.000000000000000000, 0.000000000000000000, -0.000000000000000000 ) ) ;
#867 = CIRCLE ( 'NONE', #238, 4.000000000000021316 ) ;
#868 = AXIS2_PLACEMENT_3D ( 'NONE', #16000, #8438, #3843 ) ;
#869 = VERTEX_POINT ( 'NONE', #18994 ) ;
#870 = VERTEX_POINT ( 'NONE', #11414 ) ;
#871 = FACE_OUTER_BOUND ( 'NONE', #2850, .T. ) ;
#872 = VECTOR ( 'NONE', #8868, 1000.000000000000000 ) ;
#873 = DIRECTION ( 'NONE',  ( 0.000000000000000000, 0.000000000000000000, 1.000000000000000000 ) ) ;
#874 = DIRECTION ( 'NONE',  ( 0.000000000000000000, 0.000000000000000000, -1.000000000000000000 ) ) ;
#875 = ITEM_DEFINED_TRANSFORMATION ( 'NONE', 'NONE', #13244,  #10359 ) ;
#876 = ADVANCED_FACE ( 'NONE', ( #9941 ), #2806, .F. ) ;
#877 = EDGE_LOOP ( 'NONE', ( #6023, #12373, #14389 ) ) ;
#878 = DIRECTION ( 'NONE',  ( -1.000000000000000000, 0.000000000000000000, 0.000000000000000000 ) ) ;
#879 = EDGE_LOOP ( 'NONE', ( #461, #556, #5752, #5214, #13460, #2512, #1411, #3266, #13006, #1930, #16328, #7538, #4298, #13725, #7198, #16875, #3831, #8695, #14190, #13668 ) ) ;
#880 = EDGE_CURVE ( 'NONE', #17434, #10530, #14790, .T. ) ;
#881 = VECTOR ( 'NONE', #3136, 1000.000000000000000 ) ;
#882 = CARTESIAN_POINT ( 'NONE',  ( -8.134732861515892921, -38.27090915285207018, -9.000000000000000000 ) ) ;
#883 = EDGE_CURVE ( 'NONE', #9304, #15612, #704, .T. ) ;
#884 = DIRECTION ( 'NONE',  ( 1.000000000000000000, 0.000000000000000000, 0.000000000000000000 ) ) ;
#885 = LINE ( 'NONE', #19147, #6712 ) ;
#886 = EDGE_CURVE ( 'NONE', #11065, #15857, #4172, .T. ) ;
#887 = DIRECTION ( 'NONE',  ( -0.000000000000000000, -0.000000000000000000, 1.000000000000000000 ) ) ;
#888 = CARTESIAN_POINT ( 'NONE',  ( 44.88205777487398507, 51.19948385550240744, -3.688883143319540814 ) ) ;
#889 = CARTESIAN_POINT ( 'NONE',  ( 7.336184427528458230, 0.000000000000000000, -8.105212085995399107 ) ) ;
#890 = CARTESIAN_POINT ( 'NONE',  ( 44.03140696652192787, 47.19948385550240744, -4.306917132069425058 ) ) ;
#891 = CARTESIAN_POINT ( 'NONE',  ( 41.58830220609386430, 46.00051614449764514, -0.02388180880514929535 ) ) ;
#892 = EDGE_CURVE ( 'NONE', #16569, #17921, #12589, .T. ) ;
#893 = EDGE_CURVE ( 'NONE', #7333, #12819, #16525, .T. ) ;
#894 = CARTESIAN_POINT ( 'NONE',  ( -2.499999999999999556, 3.061616997868382648E-16, 3.469446951953614189E-15 ) ) ;
#895 = DIRECTION ( 'NONE',  ( 0.1305261922200524338, 0.9914448613738102711, 0.000000000000000000 ) ) ;
#896 = AXIS2_PLACEMENT_3D ( 'NONE', #10269, #16272, #2847 ) ;
#897 = CIRCLE ( 'NONE', #2165, 1.535500000000000087 ) ;
#898 = CARTESIAN_POINT ( 'NONE',  ( 0.000000000000000000, 0.000000000000000000, 0.000000000000000000 ) ) ;
#899 = ORIENTED_EDGE ( 'NONE', *, *, #10276, .F. ) ;
#900 = CARTESIAN_POINT ( 'NONE',  ( 1.566204647097437341, -6.822536405429464601, -0.8000000000000000444 ) ) ;
#901 = CARTESIAN_POINT ( 'NONE',  ( -1.150000000000000577, 0.000000000000000000, 0.000000000000000000 ) ) ;
#902 = CARTESIAN_POINT ( 'NONE',  ( 43.34962307344078880, 52.10051614449766078, -2.184720259617096705 ) ) ;
#903 = ADVANCED_FACE ( 'NONE', ( #342 ), #236, .F. ) ;
#904 = DIRECTION ( 'NONE',  ( 1.000000000000000000, 0.000000000000000000, 0.000000000000000000 ) ) ;
#905 = ADVANCED_FACE ( 'NONE', ( #9056 ), #10327, .F. ) ;
#906 = CARTESIAN_POINT ( 'NONE',  ( 4.211140560182196957, -2.431303136016555122, -3.745885042887436622 ) ) ;
#907 = ORIENTED_EDGE ( 'NONE', *, *, #11164, .T. ) ;
#908 = CARTESIAN_POINT ( 'NONE',  ( 4.180345304246197990, -2.049116244671341569, 3.591763845239312136 ) ) ;
#909 = AXIS2_PLACEMENT_3D ( 'NONE', #9474, #8004, #12326 ) ;
#910 = CARTESIAN_POINT ( 'NONE',  ( -13.86289650954781649, -33.38261212717723936, 9.000000000000000000 ) ) ;
#911 = CIRCLE ( 'NONE', #12183, 20.00000000000000000 ) ;
#912 = DIRECTION ( 'NONE',  ( 0.000000000000000000, 0.000000000000000000, 1.000000000000000000 ) ) ;
#913 = CARTESIAN_POINT ( 'NONE',  ( 44.03140696652192787, 49.19948385550240033, -4.306917132069425058 ) ) ;
#914 = CARTESIAN_POINT ( 'NONE',  ( 14.86289650954800479, -33.38261212717704041, 9.000000000000000000 ) ) ;
#915 = CARTESIAN_POINT ( 'NONE',  ( 56.81924384183011512, 50.19948385550241454, 4.924951120819313743 ) ) ;
#916 = DIRECTION ( 'NONE',  ( -0.000000000000000000, 0.000000000000000000, -1.000000000000000000 ) ) ;
#917 = CARTESIAN_POINT ( 'NONE',  ( 49.97728705011494554, 59.50051614449765935, 6.000000000000000888 ) ) ;
#918 = AXIS2_PLACEMENT_3D ( 'NONE', #15707, #18757, #14119 ) ;
#919 = PLANE ( 'NONE',  #15371 ) ;
#920 = CARTESIAN_POINT ( 'NONE',  ( 13.61000000000001009, 0.000000000000000000, 2.000000000000001332 ) ) ;
#921 = EDGE_LOOP ( 'NONE', ( #10443, #9590, #15952, #12832 ) ) ;
#922 = ORIENTED_EDGE ( 'NONE', *, *, #17197, .T. ) ;
#923 = FACE_BOUND ( 'NONE', #14792, .T. ) ;
#924 = ORIENTED_EDGE ( 'NONE', *, *, #9379, .T. ) ;
#925 = CIRCLE ( 'NONE', #14378, 5.000000000000000888 ) ;
#926 = VECTOR ( 'NONE', #18447, 1000.000000000000000 ) ;
#927 = DIRECTION ( 'NONE',  ( -0.000000000000000000, -0.000000000000000000, -1.000000000000000000 ) ) ;
#928 = VERTEX_POINT ( 'NONE', #1810 ) ;
#929 = FACE_BOUND ( 'NONE', #9121, .T. ) ;
#930 = ADVANCED_FACE ( 'NONE', ( #3195 ), #3277, .F. ) ;
#931 = CARTESIAN_POINT ( 'NONE',  ( 55.94051828345050836, 55.79948385550239465, -4.345558710429103577 ) ) ;
#932 = ORIENTED_EDGE ( 'NONE', *, *, #15552, .T. ) ;
#933 = VECTOR ( 'NONE', #904, 1000.000000000000000 ) ;
#934 = EDGE_CURVE ( 'NONE', #17942, #4148, #5717, .T. ) ;
#935 = LINE ( 'NONE', #14456, #16661 ) ;
#936 = EDGE_LOOP ( 'NONE', ( #5155, #11862, #5868, #11722 ) ) ;
#937 = CARTESIAN_POINT ( 'NONE',  ( 54.72065718078924590, 60.29948385550240175, 6.458785618021043895 ) ) ;
#938 = CARTESIAN_POINT ( 'NONE',  ( 2.171643655288379993, -3.365003104552334978, -1.195831703456429434E-14 ) ) ;
#939 = CARTESIAN_POINT ( 'NONE',  ( 55.08986747509847248, 49.79948385550240175, -3.727524721679197572 ) ) ;
#940 = ADVANCED_FACE ( 'NONE', ( #4362, #16332 ), #1714, .T. ) ;
#941 = LINE ( 'NONE', #10137, #9151 ) ;
#942 = DIRECTION ( 'NONE',  ( 0.000000000000000000, 8.673617379884036458E-16, 1.000000000000000000 ) ) ;
#943 = CARTESIAN_POINT ( 'NONE',  ( 57.61547081786810764, 46.90051614449766504, -2.450534656007114176 ) ) ;
#944 = VECTOR ( 'NONE', #12350, 999.9999999999998863 ) ;
#945 = CARTESIAN_POINT ( 'NONE',  ( 55.71335778527780036, 44.90051614449765793, -1.832500667257213056 ) ) ;
#946 = CARTESIAN_POINT ( 'NONE',  ( -9.999999999999998224, 15.00000000000001776, -9.999999999999998224 ) ) ;
#947 = CARTESIAN_POINT ( 'NONE',  ( 1.250000000000001110, 0.000000000000000000, -5.400000000000000355 ) ) ;
#948 = EDGE_LOOP ( 'NONE', ( #5660, #14767, #16075, #4087 ) ) ;
#949 = VECTOR ( 'NONE', #14949, 1000.000000000000000 ) ;
#950 = VERTEX_POINT ( 'NONE', #2906 ) ;
#951 = LINE ( 'NONE', #6923, #5911 ) ;
#952 = EDGE_LOOP ( 'NONE', ( #16267, #2936 ) ) ;
#953 = EDGE_CURVE ( 'NONE', #5878, #5734, #2284, .T. ) ;
#954 = CARTESIAN_POINT ( 'NONE',  ( 54.13287192849676188, 60.29948385550240886, 5.649768623646098220 ) ) ;
#955 = CYLINDRICAL_SURFACE ( 'NONE', #18451, 2.649999999999985700 ) ;
#956 = ORIENTED_EDGE ( 'NONE', *, *, #13692, .F. ) ;
#957 = ORIENTED_EDGE ( 'NONE', *, *, #12323, .T. ) ;
#958 = CARTESIAN_POINT ( 'NONE',  ( -19.97007065299861850, -18.90625500492883759, 0.000000000000000000 ) ) ;
#959 = VECTOR ( 'NONE', #17165, 1000.000000000000000 ) ;
#960 = EDGE_CURVE ( 'NONE', #12436, #2436, #8867, .T. ) ;
#961 = ORIENTED_EDGE ( 'NONE', *, *, #7036, .F. ) ;
#962 = AXIS2_PLACEMENT_3D ( 'NONE', #2262, #11249, #866 ) ;
#963 = CARTESIAN_POINT ( 'NONE',  ( -1.149999999999998135, 0.000000000000000000, 0.000000000000000000 ) ) ;
#964 = VECTOR ( 'NONE', #1344, 1000.000000000000000 ) ;
#965 = VERTEX_POINT ( 'NONE', #13662 ) ;
#966 = CARTESIAN_POINT ( 'NONE',  ( 56.66441430157296821, 54.09948385550240602, 2.141517661632100111 ) ) ;
#967 = DIRECTION ( 'NONE',  ( 9.858538378746663627E-23, -5.031452844637890958E-23, 1.000000000000000000 ) ) ;
#968 = CARTESIAN_POINT ( 'NONE',  ( 44.05948171654945611, 46.20051614449766930, -4.345558710429044069 ) ) ;
#969 = LINE ( 'NONE', #768, #15487 ) ;
#970 = CARTESIAN_POINT ( 'NONE',  ( 1.925929944387235853E-31, 15.00000000000001599, 9.999999999999998224 ) ) ;
#971 = FACE_OUTER_BOUND ( 'NONE', #8611, .T. ) ;
#972 = AXIS2_PLACEMENT_3D ( 'NONE', #4310, #13228, #1180 ) ;
#973 = AXIS2_PLACEMENT_3D ( 'NONE', #7810, #1839, #2128 ) ;
#974 = VECTOR ( 'NONE', #17216, 1000.000000000000000 ) ;
#975 = ORIENTED_EDGE ( 'NONE', *, *, #9791, .F. ) ;
#976 = VERTEX_POINT ( 'NONE', #18201 ) ;
#977 = DIRECTION ( 'NONE',  ( -1.000000000000000000, 0.000000000000000000, 0.000000000000000000 ) ) ;
#978 =( NAMED_UNIT ( * ) SI_UNIT ( $, .STERADIAN. ) SOLID_ANGLE_UNIT ( ) );
#979 = AXIS2_PLACEMENT_3D ( 'NONE', #2910, #7500, #10431 ) ;
#980 = FACE_OUTER_BOUND ( 'NONE', #485, .T. ) ;
#981 = LINE ( 'NONE', #18936, #3407 ) ;
#982 = CONTEXT_DEPENDENT_SHAPE_REPRESENTATION ( #2025, #11640 ) ;
#983 = VERTEX_POINT ( 'NONE', #10427 ) ;
#984 = CARTESIAN_POINT ( 'NONE',  ( 6.507056315241515954, 5.826803161468471437, -0.09231912136634902455 ) ) ;
#985 = EDGE_LOOP ( 'NONE', ( #10470, #4595, #111, #14625 ) ) ;
#986 = ORIENTED_EDGE ( 'NONE', *, *, #18591, .F. ) ;
#987 = CARTESIAN_POINT ( 'NONE',  ( -44.99999999999997158, -40.00000000000000000, -20.00000000000000000 ) ) ;
#988 = CARTESIAN_POINT ( 'NONE',  ( 4.151274195509680354, 4.079825909417489349, 1.184320329358001550E-15 ) ) ;
#989 = CIRCLE ( 'NONE', #8166, 5.575000000000000178 ) ;
#990 = AXIS2_PLACEMENT_3D ( 'NONE', #4540, #31, #11978 ) ;
#991 = CARTESIAN_POINT ( 'NONE',  ( 50.02271294988506156, 44.50051614449765935, -6.000000000000000888 ) ) ;
#992 = DIRECTION ( 'NONE',  ( 0.000000000000000000, 1.000000000000000000, 0.000000000000000000 ) ) ;
#993 = CARTESIAN_POINT ( 'NONE',  ( 1.398397006336996817, -6.091550361990593743, 0.000000000000000000 ) ) ;
#994 = VECTOR ( 'NONE', #12505, 999.9999999999998863 ) ;
#995 = CARTESIAN_POINT ( 'NONE',  ( 44.91013252490152752, 52.79948385550240175, 3.727524721679198461 ) ) ;
#996 = CARTESIAN_POINT ( 'NONE',  ( 0.000000000000000000, 0.000000000000000000, -5.000000000000000888 ) ) ;
#997 = CARTESIAN_POINT ( 'NONE',  ( 43.18075615816989199, 63.19948385550240744, -4.924951120819313743 ) ) ;
#998 = CARTESIAN_POINT ( 'NONE',  ( 56.81924384183006538, 48.80051614449767072, -4.924951120819380357 ) ) ;
#999 = CARTESIAN_POINT ( 'NONE',  ( -4.999999999999998224, -20.00000000000000000, 15.00000000000000355 ) ) ;
#1000 = DIRECTION ( 'NONE',  ( 1.000000000000000000, 0.000000000000000000, 0.000000000000000000 ) ) ;
#1001 = EDGE_CURVE ( 'NONE', #7143, #16099, #3099, .T. ) ;
#1002 = CARTESIAN_POINT ( 'NONE',  ( -20.00000000000000000, -19.99999999999999289, -27.00000000000000355 ) ) ;
#1003 = ORIENTED_EDGE ( 'NONE', *, *, #7597, .F. ) ;
#1004 = PRODUCT_RELATED_PRODUCT_CATEGORY ( 'part', '', ( #4453 ) ) ;
#1005 = DIRECTION ( 'NONE',  ( 1.000000000000000000, 0.000000000000000000, -0.000000000000000000 ) ) ;
#1006 = ADVANCED_FACE ( 'NONE', ( #11896, #16716 ), #7399, .T. ) ;
#1007 = CIRCLE ( 'NONE', #7575, 0.7499999999999997780 ) ;
#1008 = DIRECTION ( 'NONE',  ( 0.8191520442889875797, 0.000000000000000000, 0.5735764363510522656 ) ) ;
#1009 = CARTESIAN_POINT ( 'NONE',  ( 50.02271294988505446, 54.50051614449765935, -7.000000000000000888 ) ) ;
#1010 = EDGE_CURVE ( 'NONE', #13080, #4857, #251, .T. ) ;
#1011 = EDGE_CURVE ( 'NONE', #88, #15786, #6202, .T. ) ;
#1012 = LINE ( 'NONE', #8840, #1882 ) ;
#1013 = DIRECTION ( 'NONE',  ( 0.000000000000000000, 0.8660254037844380415, -0.5000000000000012212 ) ) ;
#1014 = VERTEX_POINT ( 'NONE', #52 ) ;
#1015 = FACE_OUTER_BOUND ( 'NONE', #18810, .T. ) ;
#1016 = ADVANCED_FACE ( 'NONE', ( #6034, #11998 ), #10619, .T. ) ;
#1017 = CARTESIAN_POINT ( 'NONE',  ( 1.390230914382191596, 4.043987460488659202, -3.502507215260488582 ) ) ;
#1018 = CARTESIAN_POINT ( 'NONE',  ( 57.36023556966787851, 49.99948385550238328, -0.02388180880522424582 ) ) ;
#1019 = DIRECTION ( 'NONE',  ( -0.000000000000000000, -0.000000000000000000, -1.000000000000000000 ) ) ;
#1020 = CARTESIAN_POINT ( 'NONE',  ( 49.97728705011495265, 63.50051614449765935, 8.000000000000001776 ) ) ;
#1021 = CARTESIAN_POINT ( 'NONE',  ( -4.024497503033519941, 2.323544716729375459, -3.572167766733379768 ) ) ;
#1022 = CARTESIAN_POINT ( 'NONE',  ( 47.74827507625469281, 48.40051614449764372, -7.007379884777203749 ) ) ;
#1023 = DIRECTION ( 'NONE',  ( 0.000000000000000000, 0.000000000000000000, 1.000000000000000000 ) ) ;
#1024 =( REPRESENTATION_RELATIONSHIP ('NONE','NONE', #16703, #1297 ) REPRESENTATION_RELATIONSHIP_WITH_TRANSFORMATION ( #14196 )SHAPE_REPRESENTATION_RELATIONSHIP( ) );
#1025 = CARTESIAN_POINT ( 'NONE',  ( 6.390820551024316565, -3.013776919160863876, 4.999999999999999112 ) ) ;
#1027 = ORIENTED_EDGE ( 'NONE', *, *, #13929, .F. ) ;
#1026 = EDGE_CURVE ( 'NONE', #2792, #1052, #11194, .T. ) ;
#1028 = EDGE_CURVE ( 'NONE', #7000, #18623, #12094, .T. ) ;
#1029 = VERTEX_POINT ( 'NONE', #10903 ) ;
#1030 = DIRECTION ( 'NONE',  ( 0.000000000000000000, 0.000000000000000000, -1.000000000000000000 ) ) ;
#1031 = VERTEX_POINT ( 'NONE', #3755 ) ;
#1032 = CARTESIAN_POINT ( 'NONE',  ( 6.534838248920896930, -2.951765777552406878, 5.112608298763836601 ) ) ;
#1033 = EDGE_LOOP ( 'NONE', ( #9433, #14051, #16065, #10439 ) ) ;
#1034 = DIRECTION ( 'NONE',  ( 0.000000000000000000, 0.000000000000000000, -1.000000000000000000 ) ) ;
#1035 = CARTESIAN_POINT ( 'NONE',  ( 44.03140696652193498, 57.19948385550239323, -4.306917132069424170 ) ) ;
#1036 = ORIENTED_EDGE ( 'NONE', *, *, #11412, .T. ) ;
#1037 = CARTESIAN_POINT ( 'NONE',  ( -154.9999999999999716, -14.99999999999999645, 15.79999999999999893 ) ) ;
#1038 = PRODUCT_DEFINITION_FORMATION_WITH_SPECIFIED_SOURCE ( 'ANY', '', #17923, .NOT_KNOWN. ) ;
#1039 = ORIENTED_EDGE ( 'NONE', *, *, #14682, .T. ) ;
#1040 = CARTESIAN_POINT ( 'NONE',  ( 47.37792948025162332, 59.39948385550240317, -7.992620115222770494 ) ) ;
#1041 = CARTESIAN_POINT ( 'NONE',  ( 2.000000000000005329, -3.464101615137751722, 0.000000000000000000 ) ) ;
#1042 = CARTESIAN_POINT ( 'NONE',  ( 49.97728705011488870, 51.49948385550240459, -6.000000000000000888 ) ) ;
#1043 = DIRECTION ( 'NONE',  ( 0.000000000000000000, 0.000000000000000000, -1.000000000000000000 ) ) ;
#1044 = DIRECTION ( 'NONE',  ( -0.9697813467099857254, -0.2439756946365076173, 1.379242460255691792E-22 ) ) ;
#1045 = CARTESIAN_POINT ( 'NONE',  ( 56.81924384183006538, 44.80051614449766362, -4.924951120819380357 ) ) ;
#1046 = CARTESIAN_POINT ( 'NONE',  ( 43.69122665457040000, 48.00051614449766646, -0.02388180880515696977 ) ) ;
#1047 = DIRECTION ( 'NONE',  ( 0.000000000000000000, 0.000000000000000000, -1.000000000000000000 ) ) ;
#1048 = CYLINDRICAL_SURFACE ( 'NONE', #2822, 7.000000000000000000 ) ;
#1049 = EDGE_LOOP ( 'NONE', ( #15031, #13226, #13310, #15158 ) ) ;
#1050 = ORIENTED_EDGE ( 'NONE', *, *, #3071, .T. ) ;
#1051 = LINE ( 'NONE', #19006, #12176 ) ;
#1052 = VERTEX_POINT ( 'NONE', #16911 ) ;
#1053 = CARTESIAN_POINT ( 'NONE',  ( 42.63976443033212860, 56.99948385550241170, 0.02388180880522514787 ) ) ;
#1054 = FILL_AREA_STYLE ('',( #14476 ) ) ;
#1055 = VERTEX_POINT ( 'NONE', #15422 ) ;
#1056 = VERTEX_POINT ( 'NONE', #15617 ) ;
#1057 = CARTESIAN_POINT ( 'NONE',  ( 2.449293598294706513E-15, -20.00000000000000000, -9.000000000000000000 ) ) ;
#1058 = ORIENTED_EDGE ( 'NONE', *, *, #752, .T. ) ;
#1059 = LINE ( 'NONE', #4191, #14747 ) ;
#1060 = ORIENTED_EDGE ( 'NONE', *, *, #4146, .T. ) ;
#1061 = CARTESIAN_POINT ( 'NONE',  ( 56.65037692655918988, 49.89948385550240317, -2.184720259617163762 ) ) ;
#1062 = CARTESIAN_POINT ( 'NONE',  ( 32.49999999999998579, 40.00000000000001421, 15.00000000000000000 ) ) ;
#1063 = CARTESIAN_POINT ( 'NONE',  ( 57.36023556966787851, 47.00051614449764514, 0.02388180880515038476 ) ) ;
#1064 = CARTESIAN_POINT ( 'NONE',  ( 0.3126073911696427010, 4.041451884327382338, -6.521455134176256610E-17 ) ) ;
#1065 = EDGE_CURVE ( 'NONE', #10087, #17459, #7878, .T. ) ;
#1066 = CARTESIAN_POINT ( 'NONE',  ( -20.00000000000000000, -19.99999999999999289, -12.00000000000000000 ) ) ;
#1067 = B_SPLINE_CURVE_WITH_KNOTS ( 'NONE', 3,
 ( #18745, #1186, #18949, #15989, #2579, #5692, #9798, #9892, #15794, #10094, #9699, #2375, #18852, #11459, #17572, #2672 ),
 .UNSPECIFIED., .F., .F.,
 ( 4, 3, 3, 3, 3, 4 ),
 ( 0.000000000000000000, 3.315506744709148100E-05, 6.608280158698798419E-05, 0.0001026520855291344940, 0.0001376952025664800986, 0.0001398064759190609653 ),
 .UNSPECIFIED. ) ;
#1068 = DIRECTION ( 'NONE',  ( 1.000000000000000000, 0.000000000000000000, 0.000000000000000000 ) ) ;
#1069 = ADVANCED_FACE ( 'NONE', ( #18387 ), #11190, .F. ) ;
#1070 = AXIS2_PLACEMENT_3D ( 'NONE', #13183, #15838, #2422 ) ;
#1071 = ORIENTED_EDGE ( 'NONE', *, *, #3385, .F. ) ;
#1072 = ORIENTED_EDGE ( 'NONE', *, *, #2201, .F. ) ;
#1073 = DIRECTION ( 'NONE',  ( 9.858538378746663627E-23, -5.031452844637890958E-23, 1.000000000000000000 ) ) ;
#1074 = VECTOR ( 'NONE', #15077, 1000.000000000000000 ) ;
#1075 = DIRECTION ( 'NONE',  ( 1.000000000000000000, 0.000000000000000000, 0.000000000000000000 ) ) ;
#1076 = SURFACE_STYLE_USAGE ( .BOTH. , #10174 ) ;
#1077 = ORIENTED_EDGE ( 'NONE', *, *, #13125, .F. ) ;
#1078 = CARTESIAN_POINT ( 'NONE',  ( 6.506891779418573662, 2.833891091414751706, 5.091556646552823473 ) ) ;
#1079 = ORIENTED_EDGE ( 'NONE', *, *, #7115, .T. ) ;
#1080 = VERTEX_POINT ( 'NONE', #8056 ) ;
#1081 = VECTOR ( 'NONE', #4236, 1000.000000000000000 ) ;
#1082 = LINE ( 'NONE', #16085, #10346 ) ;
#1083 = CARTESIAN_POINT ( 'NONE',  ( -154.9999999999999716, -14.99999999999999645, 4.000000000000000000 ) ) ;
#1084 = AXIS2_PLACEMENT_3D ( 'NONE', #18947, #19044, #14502 ) ;
#1085 = CARTESIAN_POINT ( 'NONE',  ( 44.91013252490150620, 48.20051614449766930, -3.727524721679154940 ) ) ;
#1086 = CARTESIAN_POINT ( 'NONE',  ( -19.76107906696389094, -23.08216711247160546, 0.000000000000000000 ) ) ;
#1087 = DIRECTION ( 'NONE',  ( 1.000000000000000000, 0.000000000000000000, 0.000000000000000000 ) ) ;
#1089 = CARTESIAN_POINT ( 'NONE',  ( 43.69122665457040000, 52.99948385550241170, 0.02388180880521036456 ) ) ;
#1088 = B_SPLINE_CURVE_WITH_KNOTS ( 'NONE', 3,
 ( #13468, #9047, #4255, #4650, #4459 ),
 .UNSPECIFIED., .F., .F.,
 ( 4, 1, 4 ),
 ( 0.000000000000000000, 0.002886751345948131153, 0.005773502691896262307 ),
 .UNSPECIFIED. ) ;
#1090 = CARTESIAN_POINT ( 'NONE',  ( 53.50000000000000000, 4.052968581778165278E-16, -3.309499999999999886 ) ) ;
#1091 = CARTESIAN_POINT ( 'NONE',  ( 56.66441430157296821, 46.09948385550240602, 2.141517661632100111 ) ) ;
#1092 = CARTESIAN_POINT ( 'NONE',  ( 41.58830220609386430, 48.00051614449766646, -0.02388180880514929535 ) ) ;
#1093 = CARTESIAN_POINT ( 'NONE',  ( 4.114405500665255566, -2.025575754679718177, -3.508400121684934980 ) ) ;
#1094 = CARTESIAN_POINT ( 'NONE',  ( 5.000000000000003553, -20.00000000000000000, 9.000000000000000000 ) ) ;
#1095 = DIRECTION ( 'NONE',  ( 0.000000000000000000, 0.000000000000000000, -1.000000000000000000 ) ) ;
#1096 = VERTEX_POINT ( 'NONE', #9722 ) ;
#1097 = AXIS2_PLACEMENT_3D ( 'NONE', #2260, #17352, #14186 ) ;
#1098 = CARTESIAN_POINT ( 'NONE',  ( -3.472371940586054251, -2.614027278893156669, -3.320322319202162031 ) ) ;
#1099 = DIRECTION ( 'NONE',  ( 0.000000000000000000, 0.000000000000000000, -1.000000000000000000 ) ) ;
#1100 = CARTESIAN_POINT ( 'NONE',  ( 49.97728705011495265, 51.50051614449765935, 7.000000000000000888 ) ) ;
#1101 = AXIS2_PLACEMENT_3D ( 'NONE', #11279, #9807, #15805 ) ;
#1102 = FACE_OUTER_BOUND ( 'NONE', #5429, .T. ) ;
#1103 = DIRECTION ( 'NONE',  ( 0.000000000000000000, 0.000000000000000000, -1.000000000000000000 ) ) ;
#1104 = ORIENTED_EDGE ( 'NONE', *, *, #14646, .F. ) ;
#1105 = CARTESIAN_POINT ( 'NONE',  ( -15.51323935927274711, -7.377028694403568565, -9.000000000000000000 ) ) ;
#1106 = EDGE_CURVE ( 'NONE', #13173, #8267, #17198, .T. ) ;
#1107 = CARTESIAN_POINT ( 'NONE',  ( -3.734041964264191549, -23.01611183630746638, -8.999999999999996447 ) ) ;
#1108 = CARTESIAN_POINT ( 'NONE',  ( 55.94051828345050836, 51.79948385550240175, -4.345558710429104465 ) ) ;
#1109 = DIRECTION ( 'NONE',  ( 1.000000000000000000, 0.000000000000000000, 0.000000000000000000 ) ) ;
#1110 = CARTESIAN_POINT ( 'NONE',  ( 45.31609314410967926, 46.69948385550240744, 6.485486291978119766 ) ) ;
#1111 = LINE ( 'NONE', #17781, #4763 ) ;
#1112 = CARTESIAN_POINT ( 'NONE',  ( 45.90387839640208512, 46.30051614449766362, -5.676469297603124353 ) ) ;
#1113 = DIRECTION ( 'NONE',  ( -0.000000000000000000, -0.000000000000000000, 1.000000000000000000 ) ) ;
#1114 = CIRCLE ( 'NONE', #14881, 0.9999999999999995559 ) ;
#1115 = ORIENTED_EDGE ( 'NONE', *, *, #14633, .F. ) ;
#1116 = ORIENTED_EDGE ( 'NONE', *, *, #536, .T. ) ;
#1117 = CARTESIAN_POINT ( 'NONE',  ( -31.74999999999995737, 0.000000000000000000, 0.000000000000000000 ) ) ;
#1118 = ORIENTED_EDGE ( 'NONE', *, *, #14777, .T. ) ;
#1119 = MECHANICAL_DESIGN_GEOMETRIC_PRESENTATION_REPRESENTATION (  '', ( #9556 ), #3023 ) ;
#1120 = CARTESIAN_POINT ( 'NONE',  ( 2.449293598294706513E-15, -20.00000000000000000, -20.00000000000000000 ) ) ;
#1121 = EDGE_CURVE ( 'NONE', #2436, #4796, #6494, .T. ) ;
#1122 = VERTEX_POINT ( 'NONE', #9622 ) ;
#1123 = CARTESIAN_POINT ( 'NONE',  ( 73.00000000000002842, -3.000000000000000000, 6.000000000000003553 ) ) ;
#1124 = ORIENTED_EDGE ( 'NONE', *, *, #11802, .T. ) ;
#1125 = DIRECTION ( 'NONE',  ( -0.000000000000000000, -0.000000000000000000, 1.000000000000000000 ) ) ;
#1126 = VERTEX_POINT ( 'NONE', #13937 ) ;
#1127 = CARTESIAN_POINT ( 'NONE',  ( 57.61547081786812896, 58.09948385550241312, 2.450534656007040901 ) ) ;
#1128 = CARTESIAN_POINT ( 'NONE',  ( 2.855764796983346177, -2.970025579236428737, -0.09382832055446485575 ) ) ;
#1129 = AXIS2_PLACEMENT_3D ( 'NONE', #6537, #12520, #3514 ) ;
#1130 = EDGE_CURVE ( 'NONE', #18302, #12106, #15719, .T. ) ;
#1131 = CARTESIAN_POINT ( 'NONE',  ( 55.71335778527780747, 48.09948385550240602, 1.832500667257165983 ) ) ;
#1132 = DIRECTION ( 'NONE',  ( 0.000000000000000000, 0.000000000000000000, 1.000000000000000000 ) ) ;
#1133 = EDGE_CURVE ( 'NONE', #17716, #14101, #19058, .T. ) ;
#1134 = LINE ( 'NONE', #11509, #2767 ) ;
#1135 = CARTESIAN_POINT ( 'NONE',  ( 43.20883090819742023, 50.20051614449766220, -4.963592699178938972 ) ) ;
#1136 = CARTESIAN_POINT ( 'NONE',  ( 48.07319477248762496, 50.40051614449766504, -6.007379884777208190 ) ) ;
#1137 = CIRCLE ( 'NONE', #8640, 3.500000000000000000 ) ;
#1138 = FACE_OUTER_BOUND ( 'NONE', #18234, .T. ) ;
#1139 = FACE_OUTER_BOUND ( 'NONE', #2590, .T. ) ;
#1140 = VERTEX_POINT ( 'NONE', #8159 ) ;
#1141 = EDGE_CURVE ( 'NONE', #2212, #18471, #2132, .T. ) ;
#1142 = B_SPLINE_CURVE_WITH_KNOTS ( 'NONE', 3,
 ( #10723, #1634, #9163, #12196, #15234, #6499, #1815, #10624 ),
 .UNSPECIFIED., .F., .F.,
 ( 4, 2, 2, 4 ),
 ( 0.000000000000000000, 0.002450665683189819262, 0.003675998524784728893, 0.004901331366379639391 ),
 .UNSPECIFIED. ) ;
#1143 = ORIENTED_EDGE ( 'NONE', *, *, #16287, .T. ) ;
#1144 = FACE_OUTER_BOUND ( 'NONE', #5875, .T. ) ;
#1145 = ORIENTED_EDGE ( 'NONE', *, *, #1242, .T. ) ;
#1146 = CARTESIAN_POINT ( 'NONE',  ( 43.34962307344081012, 60.89948385550241028, 2.184720259617164650 ) ) ;
#1147 = PLANE ( 'NONE',  #16880 ) ;
#1148 = ORIENTED_EDGE ( 'NONE', *, *, #1495, .F. ) ;
#1149 = ORIENTED_EDGE ( 'NONE', *, *, #15610, .T. ) ;
#1150 = CARTESIAN_POINT ( 'NONE',  ( -9.037824375505429941, -37.84146099840256738, -9.000000000000000000 ) ) ;
#1151 = DIRECTION ( 'NONE',  ( 0.000000000000000000, 0.000000000000000000, -1.000000000000000000 ) ) ;
#1152 = ORIENTED_EDGE ( 'NONE', *, *, #9150, .T. ) ;
#1153 = DIRECTION ( 'NONE',  ( 0.000000000000000000, -0.000000000000000000, -1.000000000000000000 ) ) ;
#1154 = ORIENTED_EDGE ( 'NONE', *, *, #10481, .T. ) ;
#1155 = DIRECTION ( 'NONE',  ( -9.858538378746663627E-23, 5.031452844637890958E-23, -1.000000000000000000 ) ) ;
#1156 = CARTESIAN_POINT ( 'NONE',  ( 57.36023556966787851, 51.99948385550238328, -0.02388180880522424582 ) ) ;
#1157 = ADVANCED_FACE ( 'NONE', ( #18483 ), #5123, .T. ) ;
#1158 = LINE ( 'NONE', #1450, #1173 ) ;
#1159 = VECTOR ( 'NONE', #3094, 1000.000000000000000 ) ;
#1160 = CARTESIAN_POINT ( 'NONE',  ( 54.13287192849671214, 50.70051614449766220, -5.649768623646139964 ) ) ;
#1161 = DIRECTION ( 'NONE',  ( 0.9914448613738103822, -0.1305261922200521840, 0.000000000000000000 ) ) ;
#1162 = SURFACE_SIDE_STYLE ('',( #10260 ) ) ;
#1163 = DIRECTION ( 'NONE',  ( 0.9999419836444144449, 0.01077169184824073971, -2.272467923560868285E-17 ) ) ;
#1164 = AXIS2_PLACEMENT_3D ( 'NONE', #4910, #9218, #3632 ) ;
#1165 = PRODUCT_DEFINITION_SHAPE ( 'NONE', 'NONE',  #19424 ) ;
#1166 = ORIENTED_EDGE ( 'NONE', *, *, #17313, .T. ) ;
#1167 = VERTEX_POINT ( 'NONE', #8253 ) ;
#1168 = CARTESIAN_POINT ( 'NONE',  ( 1.267864665261691752E-11, -20.00000000000000000, 9.999999999999998224 ) ) ;
#1169 = CIRCLE ( 'NONE', #13978, 5.384454397937118664 ) ;
#1170 = DIRECTION ( 'NONE',  ( 0.000000000000000000, 0.000000000000000000, -1.000000000000000000 ) ) ;
#1171 = CARTESIAN_POINT ( 'NONE',  ( -159.0000000000000000, -14.99999999999999645, -15.00000000000000000 ) ) ;
#1172 = ORIENTED_EDGE ( 'NONE', *, *, #4024, .F. ) ;
#1173 = VECTOR ( 'NONE', #10358, 1000.000000000000000 ) ;
#1174 = DIRECTION ( 'NONE',  ( -0.000000000000000000, -0.000000000000000000, 1.000000000000000000 ) ) ;
#1175 = ADVANCED_FACE ( 'NONE', ( #1910 ), #12378, .F. ) ;
#1176 = ORIENTED_EDGE ( 'NONE', *, *, #18527, .T. ) ;
#1177 =( BOUNDED_SURFACE ( )  B_SPLINE_SURFACE ( 3, 2, ( 
 ( #1025, #3764, #8259 ),
 ( #10023, #6987, #16024 ),
 ( #12680, #5618, #9629 ),
 ( #12967, #7084, #2610 ),
 ( #19077, #18681, #17108 ),
 ( #822, #15626, #6793 ) ),
 .UNSPECIFIED., .F., .F., .T. ) 
 B_SPLINE_SURFACE_WITH_KNOTS ( ( 4, 2, 4 ),
 ( 3, 3 ),
 ( 0.02367497856332483747, 0.02662799652435013376, 0.02958101448537543005 ),
 ( 0.000000000000000000, 1.000000000000000000 ),
 .UNSPECIFIED. ) 
 GEOMETRIC_REPRESENTATION_ITEM ( )  RATIONAL_B_SPLINE_SURFACE ( (
 ( 1.000000000000000000, 0.8047781226141854649, 1.000000000000000000),
 ( 1.000000000000000000, 0.8123782257049820821, 1.000000000000000000),
 ( 1.000000000000000000, 0.8190665358012705344, 1.000000000000000000),
 ( 1.000000000000000000, 0.8192358187342196896, 1.000000000000000000),
 ( 1.000000000000000000, 0.8126132506074239537, 1.000000000000000000),
 ( 1.000000000000000000, 0.8047712440299316095, 1.000000000000000000) ) ) 
 REPRESENTATION_ITEM ( '' )  SURFACE ( )  );
#1178 = ORIENTED_EDGE ( 'NONE', *, *, #4265, .F. ) ;
#1179 = EDGE_CURVE ( 'NONE', #8779, #4092, #13851, .T. ) ;
#1180 = DIRECTION ( 'NONE',  ( 1.000000000000000000, 0.000000000000000000, 0.000000000000000000 ) ) ;
#1181 = DIRECTION ( 'NONE',  ( 0.000000000000000000, 0.000000000000000000, -1.000000000000000000 ) ) ;
#1182 = AXIS2_PLACEMENT_3D ( 'NONE', #7159, #887, #17373 ) ;
#1183 = CARTESIAN_POINT ( 'NONE',  ( 44.88205777487401349, 49.80051614449765651, 3.688883143319584779 ) ) ;
#1184 = DIRECTION ( 'NONE',  ( 1.000000000000000000, 0.000000000000000000, 0.000000000000000000 ) ) ;
#1185 = VECTOR ( 'NONE', #1170, 1000.000000000000000 ) ;
#1186 = CARTESIAN_POINT ( 'NONE',  ( 4.082498951862916670, 2.020725942163688504, 3.500000000000000000 ) ) ;
#1187 = CARTESIAN_POINT ( 'NONE',  ( 53.54508667620428497, 48.29948385550240175, 4.840751629271157874 ) ) ;
#1188 = DIRECTION ( 'NONE',  ( -0.000000000000000000, 1.000000000000000000, -0.000000000000000000 ) ) ;
#1189 = MECHANICAL_DESIGN_GEOMETRIC_PRESENTATION_REPRESENTATION (  '', ( #10238 ), #17161 ) ;
#1190 = CARTESIAN_POINT ( 'NONE',  ( 52.62207051974839089, 64.39948385550239607, 7.992620115222770494 ) ) ;
#1191 = CARTESIAN_POINT ( 'NONE',  ( 47.74827507625469281, 64.40051614449765793, -7.007379884777203749 ) ) ;
#1192 = CARTESIAN_POINT ( 'NONE',  ( 4.170895651974849017, -2.054890354522642237, -3.559174498016357102 ) ) ;
#1193 = FACE_OUTER_BOUND ( 'NONE', #16326, .T. ) ;
#1194 = VECTOR ( 'NONE', #12290, 1000.000000000000000 ) ;
#1195 = ORIENTED_EDGE ( 'NONE', *, *, #3564, .F. ) ;
#1196 = DIRECTION ( 'NONE',  ( 0.9135454576426006446, 0.4067366430758008189, 0.000000000000000000 ) ) ;
#1197 = EDGE_CURVE ( 'NONE', #7823, #8408, #14228, .T. ) ;
#1198 = AXIS2_PLACEMENT_3D ( 'NONE', #1893, #7863, #13838 ) ;
#1199 = DIRECTION ( 'NONE',  ( 0.000000000000000000, -1.000000000000000000, 0.000000000000000000 ) ) ;
#1200 = CARTESIAN_POINT ( 'NONE',  ( 6.270568613849419215, -4.911887854652846386, -1.704496029161938875 ) ) ;
#1201 = CARTESIAN_POINT ( 'NONE',  ( 19.97007065299861139, -18.90625500492856759, 9.000000000000000000 ) ) ;
#1202 = VERTEX_POINT ( 'NONE', #9438 ) ;
#1203 = DIRECTION ( 'NONE',  ( 0.000000000000000000, 0.000000000000000000, -1.000000000000000000 ) ) ;
#1204 = CARTESIAN_POINT ( 'NONE',  ( -154.9999999999999716, -14.99999999999999645, -15.00000000000000000 ) ) ;
#1205 = CARTESIAN_POINT ( 'NONE',  ( 43.34962307344081012, 50.89948385550241028, 2.184720259617164650 ) ) ;
#1206 = DIRECTION ( 'NONE',  ( 0.000000000000000000, 0.000000000000000000, 1.000000000000000000 ) ) ;
#1207 = CARTESIAN_POINT ( 'NONE',  ( 54.72065718078924590, 46.29948385550240886, 6.458785618021043895 ) ) ;
#1208 = CARTESIAN_POINT ( 'NONE',  ( -4.101948962585906244, 2.368261337751074169, -3.681124513963621503 ) ) ;
#1209 = CARTESIAN_POINT ( 'NONE',  ( 55.96859303347802239, 46.80051614449767072, -4.306917132069484566 ) ) ;
#1210 = AXIS2_PLACEMENT_3D ( 'NONE', #7268, #4223, #10291 ) ;
#1211 = CARTESIAN_POINT ( 'NONE',  ( -1.249999999999997558, 0.000000000000000000, -4.599999999999999645 ) ) ;
#1212 = ORIENTED_EDGE ( 'NONE', *, *, #16769, .F. ) ;
#1213 = PRESENTATION_LAYER_ASSIGNMENT (  '', '', ( #14359 ) ) ;
#1214 = ORIENTED_EDGE ( 'NONE', *, *, #7806, .F. ) ;
#1215 = CARTESIAN_POINT ( 'NONE',  ( 3.309651814758564736, -5.455921364805393026, 0.000000000000000000 ) ) ;
#1216 = ORIENTED_EDGE ( 'NONE', *, *, #14103, .F. ) ;
#1217 = DIRECTION ( 'NONE',  ( 0.000000000000000000, 1.000000000000000000, 0.000000000000000000 ) ) ;
#1218 = EDGE_LOOP ( 'NONE', ( #16081, #537, #7795, #14958 ) ) ;
#1219 = CARTESIAN_POINT ( 'NONE',  ( -62.49999999999997158, 32.50000000000001421, -9.999999999999998224 ) ) ;
#1220 = VECTOR ( 'NONE', #3702, 1000.000000000000000 ) ;
#1221 = AXIS2_PLACEMENT_3D ( 'NONE', #12128, #15173, #18237 ) ;
#1222 = EDGE_LOOP ( 'NONE', ( #4222, #8069, #18986 ) ) ;
#1223 = CARTESIAN_POINT ( 'NONE',  ( 32.00000000000000000, -1.000000000000000000, 6.000000000000001776 ) ) ;
#1224 = ORIENTED_EDGE ( 'NONE', *, *, #8355, .F. ) ;
#1225 = CARTESIAN_POINT ( 'NONE',  ( 56.79116909180255135, 61.79948385550240175, -4.963592699179005585 ) ) ;
#1226 = DIRECTION ( 'NONE',  ( 0.000000000000000000, -0.5000000000000011102, -0.8660254037844380415 ) ) ;
#1227 = B_SPLINE_CURVE_WITH_KNOTS ( 'NONE', 3,
 ( #18034, #4596, #1560, #11644, #4300 ),
 .UNSPECIFIED., .F., .F.,
 ( 4, 1, 4 ),
 ( 5.337851785822274535E-20, 0.002020725942163691374, 0.004041451884327382747 ),
 .UNSPECIFIED. ) ;
#1228 = CARTESIAN_POINT ( 'NONE',  ( 48.02776887271745210, 51.39948385550241028, -5.992620115222778487 ) ) ;
#1229 = CARTESIAN_POINT ( 'NONE',  ( -158.9999999999999716, -14.99999999999999645, 15.00000000000000000 ) ) ;
#1230 = CARTESIAN_POINT ( 'NONE',  ( -74.99999999999997158, -3.000000000000000000, 6.000000000000003553 ) ) ;
#1231 = COLOUR_RGB ( '',1.000000000000000000, 0.9490196078431372140, 0.9098039215686274384 ) ;
#1232 = CARTESIAN_POINT ( 'NONE',  ( 54.72065718078918906, 48.70051614449766930, -6.458785618021089192 ) ) ;
#1233 = CARTESIAN_POINT ( 'NONE',  ( 50.02271294988506156, 50.50051614449765935, -6.000000000000000888 ) ) ;
#1234 = CYLINDRICAL_SURFACE ( 'NONE', #12250, 20.00000000000000000 ) ;
#1235 = FACE_BOUND ( 'NONE', #16760, .T. ) ;
#1236 = VECTOR ( 'NONE', #3578, 1000.000000000000000 ) ;
#1237 = ORIENTED_EDGE ( 'NONE', *, *, #13531, .F. ) ;
#1238 = CIRCLE ( 'NONE', #3129, 5.000000000000000888 ) ;
#1239 = ORIENTED_EDGE ( 'NONE', *, *, #7238, .T. ) ;
#1240 = DIRECTION ( 'NONE',  ( 0.000000000000000000, 0.000000000000000000, 1.000000000000000000 ) ) ;
#1241 = ORIENTED_EDGE ( 'NONE', *, *, #11894, .T. ) ;
#1242 = EDGE_CURVE ( 'NONE', #14765, #10609, #3913, .T. ) ;
#1243 = CARTESIAN_POINT ( 'NONE',  ( 50.02271294988512551, 62.49948385550240459, 7.000000000000000888 ) ) ;
#1244 = CARTESIAN_POINT ( 'NONE',  ( 0.000000000000000000, 0.000000000000000000, -5.000000000000000000 ) ) ;
#1245 = CIRCLE ( 'NONE', #619, 1.999999999999998224 ) ;
#1246 = ORIENTED_EDGE ( 'NONE', *, *, #13234, .F. ) ;
#1247 = VERTEX_POINT ( 'NONE', #18585 ) ;
#1248 = CARTESIAN_POINT ( 'NONE',  ( 19.02113032590313679, -26.18033988749876428, -9.000000000000000000 ) ) ;
#1249 = DIRECTION ( 'NONE',  ( 1.000000000000000000, 0.000000000000000000, 0.000000000000000000 ) ) ;
#1250 = EDGE_CURVE ( 'NONE', #1167, #2111, #10806, .T. ) ;
#1251 = VERTEX_POINT ( 'NONE', #9338 ) ;
#1252 = DIRECTION ( 'NONE',  ( 1.000000000000000000, 0.000000000000000000, 0.000000000000000000 ) ) ;
#1253 = ORIENTED_EDGE ( 'NONE', *, *, #5246, .T. ) ;
#1254 = VECTOR ( 'NONE', #13053, 1000.000000000000000 ) ;
#1255 = CYLINDRICAL_SURFACE ( 'NONE', #14463, 1.000000000000000888 ) ;
#1256 = EDGE_CURVE ( 'NONE', #4089, #983, #12142, .T. ) ;
#1257 = EDGE_CURVE ( 'NONE', #7908, #5389, #9625, .T. ) ;
#1258 = CARTESIAN_POINT ( 'NONE',  ( 49.97728705011488159, 53.49948385550240459, -7.000000000000000888 ) ) ;
#1259 = CARTESIAN_POINT ( 'NONE',  ( -72.99999999999997158, 1.000000000000000000, 6.000000000000000000 ) ) ;
#1260 = CARTESIAN_POINT ( 'NONE',  ( 49.97728705011495265, 45.50051614449765935, 7.000000000000000888 ) ) ;
#1261 = CYLINDRICAL_SURFACE ( 'NONE', #6698, 8.000000000000007105 ) ;
#1262 = EDGE_CURVE ( 'NONE', #6920, #5143, #18873, .T. ) ;
#1263 = VECTOR ( 'NONE', #13574, 1000.000000000000000 ) ;
#1264 = DIRECTION ( 'NONE',  ( 1.000000000000000000, 0.000000000000000000, 0.000000000000000000 ) ) ;
#1265 = ORIENTED_EDGE ( 'NONE', *, *, #11172, .F. ) ;
#1266 = VERTEX_POINT ( 'NONE', #5715 ) ;
#1267 = PLANE ( 'NONE',  #8389 ) ;
#1268 = SURFACE_STYLE_FILL_AREA ( #16078 ) ;
#1269 = CIRCLE ( 'NONE', #13151, 1.000000000000001554 ) ;
#1270 = ADVANCED_FACE ( 'NONE', ( #12871 ), #4238, .T. ) ;
#1271 = B_SPLINE_CURVE_WITH_KNOTS ( 'NONE', 3,
 ( #7672, #13653, #4648, #7869, #133, #3464, #3364, #1704, #12462, #15320, #13842, #18473, #9045, #10608, #3088, #16902 ),
 .UNSPECIFIED., .F., .F.,
 ( 4, 3, 3, 3, 3, 4 ),
 ( -2.669610558406242719E-06, 0.000000000000000000, 5.703179328865551904E-05, 0.0001157653700805886653, 0.0001686517580799675017, 0.0002219032271235110720 ),
 .UNSPECIFIED. ) ;
#1272 = DIRECTION ( 'NONE',  ( 1.000000000000000000, 0.000000000000000000, 0.000000000000000000 ) ) ;
#1273 = EDGE_CURVE ( 'NONE', #8664, #2509, #17299, .T. ) ;
#1274 = CARTESIAN_POINT ( 'NONE',  ( 75.00000000000002842, -39.99999999999998579, 10.00000000000000000 ) ) ;
#1275 = AXIS2_PLACEMENT_3D ( 'NONE', #4500, #177, #5766 ) ;
#1276 = EDGE_LOOP ( 'NONE', ( #15528, #6935, #13268, #10192 ) ) ;
#1277 = CARTESIAN_POINT ( 'NONE',  ( -155.0712099064782876, -18.99936609342274707, -15.79999999999999538 ) ) ;
#1278 = AXIS2_PLACEMENT_3D ( 'NONE', #9226, #5014, #3552 ) ;
#1279 = ORIENTED_EDGE ( 'NONE', *, *, #7480, .T. ) ;
#1280 = ORIENTED_EDGE ( 'NONE', *, *, #2081, .T. ) ;
#1281 = CARTESIAN_POINT ( 'NONE',  ( -62.49999999999997158, 32.50000000000001421, 9.999999999999998224 ) ) ;
#1282 = DIRECTION ( 'NONE',  ( 1.000000000000000000, 0.000000000000000000, 0.000000000000000000 ) ) ;
#1284 = AXIS2_PLACEMENT_3D ( 'NONE', #12742, #14108, #3631 ) ;
#1283 = CARTESIAN_POINT ( 'NONE',  ( 44.30067958973594955, 50.10051614449766078, -1.875703265242155693 ) ) ;
#1285 = DIRECTION ( 'NONE',  ( -1.000000000000000000, -0.000000000000000000, -0.000000000000000000 ) ) ;
#1286 = CARTESIAN_POINT ( 'NONE',  ( 0.000000000000000000, 0.4273491293402468805, -0.8000000000000000444 ) ) ;
#1287 = CARTESIAN_POINT ( 'NONE',  ( 49.97728705011488870, 51.49948385550240459, -6.000000000000000888 ) ) ;
#1288 = CIRCLE ( 'NONE', #12233, 0.9999999999999995559 ) ;
#1289 = CARTESIAN_POINT ( 'NONE',  ( 2.712762565639649015, -3.052587955997662306, -3.430618716626630871 ) ) ;
#1290 = AXIS2_PLACEMENT_3D ( 'NONE', #10129, #14632, #19085 ) ;
#1291 = CARTESIAN_POINT ( 'NONE',  ( 57.36023556966787851, 51.99948385550238328, -0.02388180880522424582 ) ) ;
#1292 = CARTESIAN_POINT ( 'NONE',  ( 47.42335538002180328, 46.40051614449765793, -8.007379884777206414 ) ) ;
#1293 = CARTESIAN_POINT ( 'NONE',  ( 1.249999999999997780, 0.000000000000000000, -4.100000000000000533 ) ) ;
#1294 =( GEOMETRIC_REPRESENTATION_CONTEXT ( 3 ) GLOBAL_UNCERTAINTY_ASSIGNED_CONTEXT ( ( #7918 ) ) GLOBAL_UNIT_ASSIGNED_CONTEXT ( ( #10001, #706, #6677 ) ) REPRESENTATION_CONTEXT ( 'NONE', 'WORKASPACE' ) );
#1295 = DIRECTION ( 'NONE',  ( 0.000000000000000000, 0.000000000000000000, 1.000000000000000000 ) ) ;
#1296 =( NAMED_UNIT ( * ) SI_UNIT ( $, .STERADIAN. ) SOLID_ANGLE_UNIT ( ) );
#1297 = SHAPE_REPRESENTATION ( 'hex flange bolt small_iso_ISO 4162 - M5 x 40 x 16-N', ( #10359 ), #10908 ) ;
#1298 = ORIENTED_EDGE ( 'NONE', *, *, #536, .F. ) ;
#1299 = CARTESIAN_POINT ( 'NONE',  ( -20.00000000000000000, -19.99999999999999289, -20.00000000000000000 ) ) ;
#1300 = ADVANCED_FACE ( 'NONE', ( #7077 ), #16017, .F. ) ;
#1301 = DIRECTION ( 'NONE',  ( -0.9768494444668812671, -0.2139279384389642935, 0.000000000000000000 ) ) ;
#1302 = VECTOR ( 'NONE', #12915, 1000.000000000000000 ) ;
#1303 = AXIS2_PLACEMENT_3D ( 'NONE', #18296, #7784, #10909 ) ;
#1304 = CARTESIAN_POINT ( 'NONE',  ( -3.511755186886750479, 2.826662030176366081, -3.597382984111578086 ) ) ;
#1305 = DIRECTION ( 'NONE',  ( 0.1305261922200524616, 0.9914448613738103822, -0.000000000000000000 ) ) ;
#1306 = FACE_OUTER_BOUND ( 'NONE', #16945, .T. ) ;
#1307 = DIRECTION ( 'NONE',  ( 1.000000000000000000, 0.000000000000000000, 0.000000000000000000 ) ) ;
#1308 = CARTESIAN_POINT ( 'NONE',  ( -0.1410422978106123659, 4.700232962125094893, -3.687027686973624707 ) ) ;
#1309 = CARTESIAN_POINT ( 'NONE',  ( 47.70284917648453415, 49.39948385550238896, -6.992620115222774047 ) ) ;
#1310 = CARTESIAN_POINT ( 'NONE',  ( -20.63749999999999929, 0.000000000000000000, 0.000000000000000000 ) ) ;
#1311 = CARTESIAN_POINT ( 'NONE',  ( 54.68390685589033495, 53.69948385550240744, -6.485486291978119766 ) ) ;
#1312 = CARTESIAN_POINT ( 'NONE',  ( 56.65037692655921120, 49.10051614449766078, 2.184720259617097593 ) ) ;
#1313 = EDGE_CURVE ( 'NONE', #2243, #15034, #11481, .T. ) ;
#1314 = CARTESIAN_POINT ( 'NONE',  ( 30.00000000000000000, -40.00000000000000000, 12.50000000000000000 ) ) ;
#1315 = VECTOR ( 'NONE', #1680, 1000.000000000000000 ) ;
#1316 = ORIENTED_EDGE ( 'NONE', *, *, #6301, .F. ) ;
#1317 = EDGE_CURVE ( 'NONE', #4060, #2011, #16539, .T. ) ;
#1318 =( GEOMETRIC_REPRESENTATION_CONTEXT ( 3 ) GLOBAL_UNCERTAINTY_ASSIGNED_CONTEXT ( ( #16988 ) ) GLOBAL_UNIT_ASSIGNED_CONTEXT ( ( #19323, #10363, #12122 ) ) REPRESENTATION_CONTEXT ( 'NONE', 'WORKASPACE' ) );
#1319 = ORIENTED_EDGE ( 'NONE', *, *, #16055, .T. ) ;
#1320 = CARTESIAN_POINT ( 'NONE',  ( -74.99999999999997158, -1.000000000000000000, -5.999999999999998224 ) ) ;
#1321 = VERTEX_POINT ( 'NONE', #1107 ) ;
#1322 = DIRECTION ( 'NONE',  ( 1.000000000000000000, 0.000000000000000000, 0.000000000000000000 ) ) ;
#1323 = EDGE_LOOP ( 'NONE', ( #6367, #5280, #1972, #14556 ) ) ;
#1324 = DIRECTION ( 'NONE',  ( -0.000000000000000000, -0.000000000000000000, 1.000000000000000000 ) ) ;
#1325 = ORIENTED_EDGE ( 'NONE', *, *, #14048, .F. ) ;
#1326 = CARTESIAN_POINT ( 'NONE',  ( -4.747884751462026820, -5.143694235355983579, 0.000000000000000000 ) ) ;
#1327 = EDGE_LOOP ( 'NONE', ( #17850, #7240, #8290, #4277 ) ) ;
#1328 = CARTESIAN_POINT ( 'NONE',  ( 50.02271294988513972, 58.49948385550241170, 8.000000000000001776 ) ) ;
#1329 = DIRECTION ( 'NONE',  ( 1.000000000000000000, 0.000000000000000000, 0.000000000000000000 ) ) ;
#1330 = CARTESIAN_POINT ( 'NONE',  ( 44.91013252490152752, 58.79948385550240175, 3.727524721679198461 ) ) ;
#1331 = CARTESIAN_POINT ( 'NONE',  ( -9.037824375505556063, -2.158539001597497897, 0.000000000000000000 ) ) ;
#1332 = DIRECTION ( 'NONE',  ( -1.000000000000000000, -0.000000000000000000, -0.000000000000000000 ) ) ;
#1333 = CARTESIAN_POINT ( 'NONE',  ( 43.20883090819742023, 46.20051614449766220, -4.963592699178938972 ) ) ;
#1334 = CARTESIAN_POINT ( 'NONE',  ( 44.30067958973594955, 52.10051614449766788, -1.875703265242155693 ) ) ;
#1335 = LINE ( 'NONE', #9059, #7854 ) ;
#1336 = DIRECTION ( 'NONE',  ( 1.000000000000000000, 0.000000000000000000, 0.000000000000000000 ) ) ;
#1337 = VERTEX_POINT ( 'NONE', #17596 ) ;
#1338 = AXIS2_PLACEMENT_3D ( 'NONE', #16043, #1132, #2717 ) ;
#1339 = ORIENTED_EDGE ( 'NONE', *, *, #1197, .T. ) ;
#1340 = CARTESIAN_POINT ( 'NONE',  ( 2.449293598294706513E-15, -20.00000000000000000, 9.000000000000000000 ) ) ;
#1341 = ORIENTED_EDGE ( 'NONE', *, *, #16606, .F. ) ;
#1342 = DIRECTION ( 'NONE',  ( 0.000000000000000000, -1.000000000000000000, 0.000000000000000000 ) ) ;
#1343 = VERTEX_POINT ( 'NONE', #9816 ) ;
#1344 = DIRECTION ( 'NONE',  ( 2.191393683118470056E-17, 7.538405132783724027E-17, 1.000000000000000000 ) ) ;
#1345 = CARTESIAN_POINT ( 'NONE',  ( 56.65037692655918988, 47.89948385550240317, -2.184720259617163762 ) ) ;
#1346 = ORIENTED_EDGE ( 'NONE', *, *, #10591, .T. ) ;
#1347 = CARTESIAN_POINT ( 'NONE',  ( 4.175813232069146785, 2.061359961916365613, -3.570380186727397653 ) ) ;
#1348 = ORIENTED_EDGE ( 'NONE', *, *, #12740, .T. ) ;
#1349 = CARTESIAN_POINT ( 'NONE',  ( -62.49999999999997158, 20.00000000000001421, -15.00000000000000000 ) ) ;
#1350 = CARTESIAN_POINT ( 'NONE',  ( 49.97728705011488159, 55.49948385550240459, -7.000000000000000888 ) ) ;
#1351 = LINE ( 'NONE', #1062, #18417 ) ;
#1352 = CARTESIAN_POINT ( 'NONE',  ( 44.03140696652198471, 49.80051614449766362, 4.306917132069485454 ) ) ;
#1353 = CARTESIAN_POINT ( 'NONE',  ( 32.49999999999998579, 45.00000000000001421, 5.000000000000003553 ) ) ;
#1354 = ADVANCED_FACE ( 'NONE', ( #14435 ), #4150, .F. ) ;
#1355 = DIRECTION ( 'NONE',  ( 0.3090169943749560000, -0.9510565162951507556, 0.000000000000000000 ) ) ;
#1356 = CARTESIAN_POINT ( 'NONE',  ( 6.466260427357665819, 5.808561367196023895, -1.902591328531564046E-16 ) ) ;
#1357 = DIRECTION ( 'NONE',  ( 0.000000000000000000, 0.000000000000000000, -1.000000000000000000 ) ) ;
#1358 = ORIENTED_EDGE ( 'NONE', *, *, #5669, .T. ) ;
#1359 = PRODUCT_DEFINITION ( 'UNKNOWN', '', #1975, #10856 ) ;
#1360 = ORIENTED_EDGE ( 'NONE', *, *, #9091, .F. ) ;
#1361 = ORIENTED_EDGE ( 'NONE', *, *, #9544, .T. ) ;
#1362 = FACE_OUTER_BOUND ( 'NONE', #9886, .T. ) ;
#1363 =( NAMED_UNIT ( * ) PLANE_ANGLE_UNIT ( ) SI_UNIT ( $, .RADIAN. ) );
#1364 = CARTESIAN_POINT ( 'NONE',  ( 45.27934281921075410, 63.29948385550240175, -6.458785618021043895 ) ) ;
#1365 = CARTESIAN_POINT ( 'NONE',  ( 14.17539641854901689, -5.891203581559917524, 9.000000000000000000 ) ) ;
#1366 = ORIENTED_EDGE ( 'NONE', *, *, #7879, .F. ) ;
#1367 = DIRECTION ( 'NONE',  ( 0.000000000000000000, 0.000000000000000000, -1.000000000000000000 ) ) ;
#1368 = EDGE_CURVE ( 'NONE', #3316, #16919, #2782, .T. ) ;
#1369 = ORIENTED_EDGE ( 'NONE', *, *, #5574, .F. ) ;
#1370 = ORIENTED_EDGE ( 'NONE', *, *, #9854, .F. ) ;
#1371 = DIRECTION ( 'NONE',  ( 0.000000000000000000, 0.000000000000000000, 1.000000000000000000 ) ) ;
#1372 = CARTESIAN_POINT ( 'NONE',  ( 0.3126073911696407026, -2.020725942163686728, 3.500000000000000444 ) ) ;
#1373 = CARTESIAN_POINT ( 'NONE',  ( 51.92680522751238925, 49.40051614449766504, 6.007379884777208190 ) ) ;
#1374 = DIRECTION ( 'NONE',  ( -1.000000000000000000, 0.000000000000000000, 0.000000000000000000 ) ) ;
#1375 = EDGE_CURVE ( 'NONE', #3962, #17116, #13061, .T. ) ;
#1376 = AXIS2_PLACEMENT_3D ( 'NONE', #10644, #15161, #18227 ) ;
#1377 = EDGE_CURVE ( 'NONE', #14477, #19163, #867, .T. ) ;
#1378 = CARTESIAN_POINT ( 'NONE',  ( 50.02271294988511841, 54.49948385550240459, 6.000000000000000888 ) ) ;
#1379 = DIRECTION ( 'NONE',  ( -0.000000000000000000, -0.000000000000000000, 1.000000000000000000 ) ) ;
#1380 = CARTESIAN_POINT ( 'NONE',  ( 54.13287192849676188, 50.29948385550240175, 5.649768623646098220 ) ) ;
#1381 = VECTOR ( 'NONE', #19322, 1000.000000000000000 ) ;
#1382 = CARTESIAN_POINT ( 'NONE',  ( 47.37792948025170858, 51.60051614449766788, 7.992620115222797139 ) ) ;
#1383 = CARTESIAN_POINT ( 'NONE',  ( -6.259644161404860030E-16, -4.618802153517027165, -3.433295621305388234 ) ) ;
#1384 = CARTESIAN_POINT ( 'NONE',  ( 4.086376042167605860, 1.979461949354204719, -3.571471332069177773 ) ) ;
#1385 = CYLINDRICAL_SURFACE ( 'NONE', #7142, 2.447112362156698140 ) ;
#1386 =( NAMED_UNIT ( * ) PLANE_ANGLE_UNIT ( ) SI_UNIT ( $, .RADIAN. ) );
#1387 = ADVANCED_FACE ( 'NONE', ( #17393 ), #16812, .F. ) ;
#1388 = EDGE_CURVE ( 'NONE', #18424, #2267, #13694, .T. ) ;
#1389 = ORIENTED_EDGE ( 'NONE', *, *, #18061, .F. ) ;
#1390 = DIRECTION ( 'NONE',  ( 0.000000000000000000, 0.000000000000000000, -1.000000000000000000 ) ) ;
#1391 = AXIS2_PLACEMENT_3D ( 'NONE', #3560, #9620, #15615 ) ;
#1392 = EDGE_CURVE ( 'NONE', #15249, #6396, #13991, .T. ) ;
#1393 = DIRECTION ( 'NONE',  ( 0.02857142857142857401, 0.9995917534020515305, -0.000000000000000000 ) ) ;
#1394 = APPLICATION_CONTEXT ( 'automotive_design' ) ;
#1395 = VECTOR ( 'NONE', #15016, 1000.000000000000000 ) ;
#1396 = PLANE ( 'NONE',  #9068 ) ;
#1397 = CARTESIAN_POINT ( 'NONE',  ( 0.000000000000000000, 0.000000000000000000, 5.000000000000000000 ) ) ;
#1398 = CARTESIAN_POINT ( 'NONE',  ( 2.100000000000000089, 0.000000000000000000, -0.2800830152838844622 ) ) ;
#1399 = DIRECTION ( 'NONE',  ( 0.000000000000000000, -1.000000000000000000, 0.000000000000000000 ) ) ;
#1400 = FACE_OUTER_BOUND ( 'NONE', #15730, .T. ) ;
#1401 = CARTESIAN_POINT ( 'NONE',  ( 52.25172492374522903, 57.59948385550241312, -7.007379884777225953 ) ) ;
#1402 = DIRECTION ( 'NONE',  ( 0.000000000000000000, 0.000000000000000000, 1.000000000000000000 ) ) ;
#1403 = CARTESIAN_POINT ( 'NONE',  ( 41.58830220609386430, 50.99948385550241170, 0.02388180880523263147 ) ) ;
#1404 = CARTESIAN_POINT ( 'NONE',  ( -74.99999999999997158, 32.50000000000001421, -15.00000000000000000 ) ) ;
#1405 = CARTESIAN_POINT ( 'NONE',  ( 42.63976443033212860, 50.00051614449766646, -0.02388180880514948964 ) ) ;
#1406 = CARTESIAN_POINT ( 'NONE',  ( 8.500000000000000000, 5.773502691896261751, 0.000000000000000000 ) ) ;
#1407 = VECTOR ( 'NONE', #12245, 1000.000000000000000 ) ;
#1408 = ORIENTED_EDGE ( 'NONE', *, *, #9197, .F. ) ;
#1409 = ORIENTED_EDGE ( 'NONE', *, *, #16613, .T. ) ;
#1410 = DIRECTION ( 'NONE',  ( -0.000000000000000000, -0.000000000000000000, -1.000000000000000000 ) ) ;
#1411 = ORIENTED_EDGE ( 'NONE', *, *, #17612, .T. ) ;
#1412 = AXIS2_PLACEMENT_3D ( 'NONE', #1715, #16627, #18202 ) ;
#1413 = DIRECTION ( 'NONE',  ( 0.000000000000000000, 0.000000000000000000, -1.000000000000000000 ) ) ;
#1414 = ORIENTED_EDGE ( 'NONE', *, *, #12268, .T. ) ;
#1415 = FACE_OUTER_BOUND ( 'NONE', #16823, .T. ) ;
#1416 = EDGE_CURVE ( 'NONE', #1616, #6480, #11976, .T. ) ;
#1417 = ORIENTED_EDGE ( 'NONE', *, *, #8421, .F. ) ;
#1418 = AXIS2_PLACEMENT_3D ( 'NONE', #5586, #3834, #884 ) ;
#1419 = CYLINDRICAL_SURFACE ( 'NONE', #19350, 4.872650870659752442 ) ;
#1420 = ORIENTED_EDGE ( 'NONE', *, *, #3761, .T. ) ;
#1421 = CARTESIAN_POINT ( 'NONE',  ( 0.000000000000000000, 0.000000000000000000, -4.000000000000000000 ) ) ;
#1422 = AXIS2_PLACEMENT_3D ( 'NONE', #16165, #17937, #8987 ) ;
#1423 = DIRECTION ( 'NONE',  ( -0.000000000000000000, -0.000000000000000000, -1.000000000000000000 ) ) ;
#1424 = ADVANCED_FACE ( 'NONE', ( #7376 ), #215, .F. ) ;
#1425 = CARTESIAN_POINT ( 'NONE',  ( 55.11794222512601493, 58.19948385550240744, 3.688883143319541702 ) ) ;
#1426 = CARTESIAN_POINT ( 'NONE',  ( 2.000000000000000000, 0.8865213383406715941, 1.535499999999999199 ) ) ;
#1427 = CARTESIAN_POINT ( 'NONE',  ( 2.000000000000000000, -1.329782007511007169, -0.7677499999999988223 ) ) ;
#1428 = CARTESIAN_POINT ( 'NONE',  ( 57.60143344285435774, 53.10051614449767499, 2.493737253992045044 ) ) ;
#1429 = AXIS2_PLACEMENT_3D ( 'NONE', #18167, #4723, #9307 ) ;
#1430 = CARTESIAN_POINT ( 'NONE',  ( 51.97223112728249816, 48.60051614449766788, -5.992620115222793586 ) ) ;
#1431 = CARTESIAN_POINT ( 'NONE',  ( 1.219878473194463187, -24.84890673354692936, 9.000000000000000000 ) ) ;
#1432 = LINE ( 'NONE', #11905, #949 ) ;
#1433 = VERTEX_POINT ( 'NONE', #19268 ) ;
#1434 = ORIENTED_EDGE ( 'NONE', *, *, #9969, .T. ) ;
#1435 = CYLINDRICAL_SURFACE ( 'NONE', #15616, 20.00000000000000000 ) ;
#1436 = ORIENTED_EDGE ( 'NONE', *, *, #6062, .T. ) ;
#1437 = LINE ( 'NONE', #5948, #15809 ) ;
#1438 = DIRECTION ( 'NONE',  ( 0.000000000000000000, 0.000000000000000000, 1.000000000000000000 ) ) ;
#1439 = EDGE_LOOP ( 'NONE', ( #2082, #16900, #12486, #14325 ) ) ;
#1440 = CARTESIAN_POINT ( 'NONE',  ( 3.734041964264196434, -16.98388816369253362, -8.999999999999996447 ) ) ;
#1441 = CIRCLE ( 'NONE', #8001, 0.9999999999999980016 ) ;
#1442 = CARTESIAN_POINT ( 'NONE',  ( 45.90387839640214196, 48.69948385550240744, 5.676469297603166098 ) ) ;
#1443 = ORIENTED_EDGE ( 'NONE', *, *, #14434, .F. ) ;
#1444 = DIRECTION ( 'NONE',  ( 1.000000000000000000, 0.000000000000000000, 0.000000000000000000 ) ) ;
#1445 = ORIENTED_EDGE ( 'NONE', *, *, #5447, .F. ) ;
#1446 = CARTESIAN_POINT ( 'NONE',  ( 49.97728705011486738, 49.49948385550241170, -8.000000000000001776 ) ) ;
#1447 = DIRECTION ( 'NONE',  ( 1.000000000000000000, 0.000000000000000000, 0.000000000000000000 ) ) ;
#1448 = CARTESIAN_POINT ( 'NONE',  ( 43.34962307344081012, 58.89948385550241028, 2.184720259617164650 ) ) ;
#1449 = VECTOR ( 'NONE', #9677, 1000.000000000000000 ) ;
#1450 = CARTESIAN_POINT ( 'NONE',  ( -20.63749999999999574, 0.000000000000000000, -5.400000000000000355 ) ) ;
#1451 = CARTESIAN_POINT ( 'NONE',  ( 47.74827507625469281, 54.40051614449766504, -7.007379884777203749 ) ) ;
#1452 = CARTESIAN_POINT ( 'NONE',  ( 32.49999999999998579, 5.000000000000018652, -4.999999999999996447 ) ) ;
#1453 = CYLINDRICAL_SURFACE ( 'NONE', #5994, 4.424999999999999822 ) ;
#1454 = EDGE_LOOP ( 'NONE', ( #9792, #2037 ) ) ;
#1455 = ORIENTED_EDGE ( 'NONE', *, *, #10708, .T. ) ;
#1456 = ORIENTED_EDGE ( 'NONE', *, *, #2108, .T. ) ;
#1457 = FACE_OUTER_BOUND ( 'NONE', #9301, .T. ) ;
#1458 = CARTESIAN_POINT ( 'NONE',  ( 41.58830220609386430, 64.99948385550240459, 0.02388180880523263147 ) ) ;
#1459 =( NAMED_UNIT ( * ) PLANE_ANGLE_UNIT ( ) SI_UNIT ( $, .RADIAN. ) );
#1460 = ORIENTED_EDGE ( 'NONE', *, *, #3650, .F. ) ;
#1461 = DIRECTION ( 'NONE',  ( 0.000000000000000000, 0.000000000000000000, 1.000000000000000000 ) ) ;
#1462 = VERTEX_POINT ( 'NONE', #18073 ) ;
#1463 = CARTESIAN_POINT ( 'NONE',  ( 55.94051828345054389, 61.20051614449765509, 4.345558710429044957 ) ) ;
#1464 = VERTEX_POINT ( 'NONE', #4636 ) ;
#1465 = CIRCLE ( 'NONE', #3966, 5.000000000000000888 ) ;
#1466 = CARTESIAN_POINT ( 'NONE',  ( 0.000000000000000000, 0.000000000000000000, 0.000000000000000000 ) ) ;
#1467 = UNCERTAINTY_MEASURE_WITH_UNIT (LENGTH_MEASURE( 1.000000000000000082E-05 ), #8121, 'distance_accuracy_value', 'NONE');
#1468 = CARTESIAN_POINT ( 'NONE',  ( -0.1717365941144614327, -6.008326913195983998, 0.000000000000000000 ) ) ;
#1469 = CARTESIAN_POINT ( 'NONE',  ( 53.54508667620424234, 50.70051614449766220, -4.840751629271188961 ) ) ;
#1470 = FACE_BOUND ( 'NONE', #952, .T. ) ;
#1471 = PRODUCT_DEFINITION_SHAPE ( 'NONE', 'NONE',  #12013 ) ;
#1472 = DIRECTION ( 'NONE',  ( 0.000000000000000000, 0.000000000000000000, 1.000000000000000000 ) ) ;
#1473 = CARTESIAN_POINT ( 'NONE',  ( 44.88205777487398507, 55.19948385550240744, -3.688883143319540814 ) ) ;
#1474 = CARTESIAN_POINT ( 'NONE',  ( 1.360585162435110629, -4.061296242128317857, -3.505054077164905024 ) ) ;
#1475 = CARTESIAN_POINT ( 'NONE',  ( 50.02271294988512551, 54.49948385550240459, 7.000000000000000888 ) ) ;
#1476 = CARTESIAN_POINT ( 'NONE',  ( 52.57664461997821093, 51.40051614449767214, 8.007379884777206414 ) ) ;
#1477 = CARTESIAN_POINT ( 'NONE',  ( -3.917148844556152511E-15, -4.821944789745365334, 1.648146632869001094 ) ) ;
#1478 = AXIS2_PLACEMENT_3D ( 'NONE', #7872, #4839, #2090 ) ;
#1479 = CARTESIAN_POINT ( 'NONE',  ( 2.000000000000000000, -1.773042676681341856, 2.276824562219559311E-15 ) ) ;
#1480 = ADVANCED_BREP_SHAPE_REPRESENTATION ( '', ( #8823, #10359 ), #8423 ) ;
#1481 = FACE_OUTER_BOUND ( 'NONE', #18132, .T. ) ;
#1482 = AXIS2_PLACEMENT_3D ( 'NONE', #7732, #10568, #12243 ) ;
#1483 = PRODUCT_CONTEXT ( 'NONE', #11764, 'mechanical' ) ;
#1484 = ORIENTED_EDGE ( 'NONE', *, *, #18632, .F. ) ;
#1485 = CARTESIAN_POINT ( 'NONE',  ( -62.49999999999997158, 32.50000000000001421, -15.00000000000000000 ) ) ;
#1486 = EDGE_CURVE ( 'NONE', #976, #17995, #14820, .T. ) ;
#1487 = DIRECTION ( 'NONE',  ( 1.000000000000000000, 0.000000000000000000, 0.000000000000000000 ) ) ;
#1488 = ADVANCED_FACE ( 'NONE', ( #2972 ), #16696, .T. ) ;
#1489 = AXIS2_PLACEMENT_3D ( 'NONE', #2753, #10173, #11646 ) ;
#1490 = FACE_OUTER_BOUND ( 'NONE', #10666, .T. ) ;
#1491 = CARTESIAN_POINT ( 'NONE',  ( 6.518095160331712989, 2.933089652807542524, 5.080260301817225432 ) ) ;
#1492 = AXIS2_PLACEMENT_3D ( 'NONE', #15841, #9755, #5350 ) ;
#1493 = CARTESIAN_POINT ( 'NONE',  ( -19.89043790736547379, -17.90943073464699609, -9.000000000000000000 ) ) ;
#1494 = ADVANCED_FACE ( 'NONE', ( #1400 ), #5241, .F. ) ;
#1495 = EDGE_CURVE ( 'NONE', #18325, #13768, #18729, .T. ) ;
#1496 = CARTESIAN_POINT ( 'NONE',  ( -17.32050807568879236, -10.00000000000004263, -9.000000000000000000 ) ) ;
#1497 = CARTESIAN_POINT ( 'NONE',  ( 45.86712807150323812, 57.29948385550240175, -5.649768623646098220 ) ) ;
#1498 = CARTESIAN_POINT ( 'NONE',  ( 4.000000000000000000, -2.309401076758514915, -3.433295621305383349 ) ) ;
#1499 = CARTESIAN_POINT ( 'NONE',  ( 47.37792948025162332, 53.39948385550241028, -7.992620115222770494 ) ) ;
#1500 = CARTESIAN_POINT ( 'NONE',  ( 0.000000000000000000, 0.000000000000000000, -5.000000000000000000 ) ) ;
#1501 = CARTESIAN_POINT ( 'NONE',  ( 44.03140696652198471, 51.80051614449766362, 4.306917132069485454 ) ) ;
#1502 = AXIS2_PLACEMENT_3D ( 'NONE', #10696, #16600, #13253 ) ;
#1503 = DIRECTION ( 'NONE',  ( 0.000000000000000000, 0.000000000000000000, 1.000000000000000000 ) ) ;
#1504 = ORIENTED_EDGE ( 'NONE', *, *, #16769, .T. ) ;
#1505 = VECTOR ( 'NONE', #18753, 1000.000000000000000 ) ;
#1506 = FILL_AREA_STYLE_COLOUR ( '', #10923 ) ;
#1507 = ORIENTED_EDGE ( 'NONE', *, *, #340, .F. ) ;
#1508 = ORIENTED_EDGE ( 'NONE', *, *, #886, .T. ) ;
#1509 = EDGE_CURVE ( 'NONE', #737, #8777, #5548, .T. ) ;
#1510 = ADVANCED_FACE ( 'NONE', ( #28 ), #13450, .T. ) ;
#1511 = CARTESIAN_POINT ( 'NONE',  ( -74.99999999999997158, -40.00000000000000000, -10.00000000000000000 ) ) ;
#1512 = EDGE_LOOP ( 'NONE', ( #14590, #15562, #17642, #12838 ) ) ;
#1513 = FACE_OUTER_BOUND ( 'NONE', #15002, .T. ) ;
#1514 = VERTEX_POINT ( 'NONE', #4538 ) ;
#1515 = LINE ( 'NONE', #10515, #14294 ) ;
#1516 = ORIENTED_EDGE ( 'NONE', *, *, #18984, .F. ) ;
#1517 = CARTESIAN_POINT ( 'NONE',  ( -99.99999999999997158, -14.99999999999999289, 10.00000000000000000 ) ) ;
#1518 = VECTOR ( 'NONE', #17948, 1000.000000000000000 ) ;
#1519 = FACE_OUTER_BOUND ( 'NONE', #5287, .T. ) ;
#1520 = CIRCLE ( 'NONE', #16559, 4.000000000000031086 ) ;
#1521 = CARTESIAN_POINT ( 'NONE',  ( 55.69932041026404335, 59.89948385550240317, -1.875703265242203432 ) ) ;
#1522 = DIRECTION ( 'NONE',  ( 0.000000000000000000, -1.000000000000000000, 0.000000000000000000 ) ) ;
#1523 = CYLINDRICAL_SURFACE ( 'NONE', #1412, 20.00000000000000000 ) ;
#1524 = CARTESIAN_POINT ( 'NONE',  ( 45.31609314410960820, 56.30051614449766362, -6.485486291978072693 ) ) ;
#1525 = CARTESIAN_POINT ( 'NONE',  ( 48.07319477248762496, 58.40051614449765793, -6.007379884777208190 ) ) ;
#1526 = CARTESIAN_POINT ( 'NONE',  ( 19.89043790736549155, -22.09056926535286891, 9.000000000000000000 ) ) ;
#1527 = DIRECTION ( 'NONE',  ( 1.000000000000000000, 0.000000000000000000, -0.000000000000000000 ) ) ;
#1528 = ORIENTED_EDGE ( 'NONE', *, *, #18544, .T. ) ;
#1529 = ORIENTED_EDGE ( 'NONE', *, *, #13719, .F. ) ;
#1530 = DIRECTION ( 'NONE',  ( 0.000000000000000000, 0.000000000000000000, -1.000000000000000000 ) ) ;
#1531 = EDGE_LOOP ( 'NONE', ( #1965, #8200, #6115, #16241 ) ) ;
#1532 =( GEOMETRIC_REPRESENTATION_CONTEXT ( 3 ) GLOBAL_UNCERTAINTY_ASSIGNED_CONTEXT ( ( #15377 ) ) GLOBAL_UNIT_ASSIGNED_CONTEXT ( ( #4479, #3113, #14956 ) ) REPRESENTATION_CONTEXT ( 'NONE', 'WORKASPACE' ) );
#1533 = AXIS2_PLACEMENT_3D ( 'NONE', #1751, #10657, #4699 ) ;
#1534 = DIRECTION ( 'NONE',  ( -0.000000000000000000, -0.000000000000000000, -1.000000000000000000 ) ) ;
#1535 = EDGE_CURVE ( 'NONE', #11812, #12707, #10245, .T. ) ;
#1536 = ORIENTED_EDGE ( 'NONE', *, *, #960, .F. ) ;
#1537 = DIRECTION ( 'NONE',  ( -9.710251638871371392E-17, -5.969973981896233748E-17, -1.000000000000000000 ) ) ;
#1538 = CARTESIAN_POINT ( 'NONE',  ( 43.34962307344081012, 48.89948385550240317, 2.184720259617164650 ) ) ;
#1539 = EDGE_CURVE ( 'NONE', #19206, #9345, #11488, .T. ) ;
#1540 = EDGE_LOOP ( 'NONE', ( #1152, #15028, #8656, #5746 ) ) ;
#1541 =( GEOMETRIC_REPRESENTATION_CONTEXT ( 3 ) GLOBAL_UNCERTAINTY_ASSIGNED_CONTEXT ( ( #7542 ) ) GLOBAL_UNIT_ASSIGNED_CONTEXT ( ( #16270, #1363, #17843 ) ) REPRESENTATION_CONTEXT ( 'NONE', 'WORKASPACE' ) );
#1542 = CYLINDRICAL_SURFACE ( 'NONE', #4122, 20.00000000000000000 ) ;
#1543 = ORIENTED_EDGE ( 'NONE', *, *, #11226, .F. ) ;
#1544 = CARTESIAN_POINT ( 'NONE',  ( 49.97728705011486738, 45.49948385550240459, -8.000000000000001776 ) ) ;
#1545 = FACE_OUTER_BOUND ( 'NONE', #5227, .T. ) ;
#1546 = CARTESIAN_POINT ( 'NONE',  ( 43.34962307344081012, 60.89948385550241028, 2.184720259617164650 ) ) ;
#1547 = CARTESIAN_POINT ( 'NONE',  ( 4.071447262713890680, -4.041451884327386779, 0.000000000000000000 ) ) ;
#1548 = DIRECTION ( 'NONE',  ( 0.03086419753086420623, -0.9995235871707959241, 0.000000000000000000 ) ) ;
#1549 = CARTESIAN_POINT ( 'NONE',  ( 49.97728705011495265, 51.50051614449765935, 7.000000000000000888 ) ) ;
#1550 = DIRECTION ( 'NONE',  ( -1.000000000000000000, 0.000000000000000000, 0.000000000000000000 ) ) ;
#1551 = CIRCLE ( 'NONE', #9363, 3.800000000000000266 ) ;
#1552 = AXIS2_PLACEMENT_3D ( 'NONE', #12885, #14449, #2511 ) ;
#1553 =( LENGTH_UNIT ( ) NAMED_UNIT ( * ) SI_UNIT ( .MILLI., .METRE. ) );
#1554 = CARTESIAN_POINT ( 'NONE',  ( -20.63749999999999929, 0.000000000000000000, 0.000000000000000000 ) ) ;
#1555 = VERTEX_POINT ( 'NONE', #13348 ) ;
#1556 = EDGE_CURVE ( 'NONE', #12796, #4767, #6808, .T. ) ;
#1557 =( GEOMETRIC_REPRESENTATION_CONTEXT ( 3 ) GLOBAL_UNCERTAINTY_ASSIGNED_CONTEXT ( ( #18148 ) ) GLOBAL_UNIT_ASSIGNED_CONTEXT ( ( #18375, #4921, #15504 ) ) REPRESENTATION_CONTEXT ( 'NONE', 'WORKASPACE' ) );
#1558 = ORIENTED_EDGE ( 'NONE', *, *, #15871, .T. ) ;
#1559 = ORIENTED_EDGE ( 'NONE', *, *, #7937, .F. ) ;
#1560 = CARTESIAN_POINT ( 'NONE',  ( 3.806834918298644954, 3.031088913245535199, -1.749999999999998446 ) ) ;
#1561 =( NAMED_UNIT ( * ) SI_UNIT ( $, .STERADIAN. ) SOLID_ANGLE_UNIT ( ) );
#1562 = EDGE_CURVE ( 'NONE', #5733, #14876, #16310, .T. ) ;
#1563 = CARTESIAN_POINT ( 'NONE',  ( 52.29715082351547295, 46.39948385550240317, 6.992620115222774047 ) ) ;
#1564 = DIRECTION ( 'NONE',  ( -1.000000000000000000, 0.000000000000000000, 0.000000000000000000 ) ) ;
#1565 = VERTEX_POINT ( 'NONE', #4445 ) ;
#1566 = CARTESIAN_POINT ( 'NONE',  ( 4.000000000000003553, 0.000000000000000000, 3.500000000000000000 ) ) ;
#1567 = AXIS2_PLACEMENT_3D ( 'NONE', #6482, #12664, #14320 ) ;
#1568 = AXIS2_PLACEMENT_3D ( 'NONE', #1117, #12971, #18979 ) ;
#1569 = VERTEX_POINT ( 'NONE', #16405 ) ;
#1570 = CARTESIAN_POINT ( 'NONE',  ( 55.96859303347802239, 58.80051614449765651, -4.306917132069484566 ) ) ;
#1571 = EDGE_LOOP ( 'NONE', ( #18455, #8024, #11206, #15769 ) ) ;
#1572 = DIRECTION ( 'NONE',  ( 0.000000000000000000, 0.000000000000000000, -1.000000000000000000 ) ) ;
#1573 = CARTESIAN_POINT ( 'NONE',  ( -1.372193374551966155E-15, -2.859595677584338969, 2.047034997319577609 ) ) ;
#1574 = CARTESIAN_POINT ( 'NONE',  ( 53.50833635130544508, 55.30051614449765651, 4.867452303228181343 ) ) ;
#1575 = FACE_BOUND ( 'NONE', #7460, .T. ) ;
#1576 = DIRECTION ( 'NONE',  ( 1.000000000000000000, 0.000000000000000000, 0.000000000000000000 ) ) ;
#1577 = CARTESIAN_POINT ( 'NONE',  ( 55.08986747509847248, 55.79948385550239465, -3.727524721679197572 ) ) ;
#1578 = CARTESIAN_POINT ( 'NONE',  ( -0.9999999999999976685, -20.00000000000000000, 8.999999999999998224 ) ) ;
#1579 = CIRCLE ( 'NONE', #3765, 4.000000000000000000 ) ;
#1580 = CARTESIAN_POINT ( 'NONE',  ( 56.81924384183006538, 50.80051614449766362, -4.924951120819380357 ) ) ;
#1581 = LINE ( 'NONE', #10578, #15025 ) ;
#1582 = FACE_OUTER_BOUND ( 'NONE', #11524, .T. ) ;
#1583 = CIRCLE ( 'NONE', #332, 2.149999999999999023 ) ;
#1584 = ORIENTED_EDGE ( 'NONE', *, *, #9029, .F. ) ;
#1585 = FACE_OUTER_BOUND ( 'NONE', #1531, .T. ) ;
#1586 =( NAMED_UNIT ( * ) PLANE_ANGLE_UNIT ( ) SI_UNIT ( $, .RADIAN. ) );
#1587 = PRODUCT_CONTEXT ( 'NONE', #4879, 'mechanical' ) ;
#1588 = VECTOR ( 'NONE', #1817, 1000.000000000000000 ) ;
#1589 = ORIENTED_EDGE ( 'NONE', *, *, #12157, .F. ) ;
#1590 = DIRECTION ( 'NONE',  ( -1.000000000000000000, -0.000000000000000000, -0.000000000000000000 ) ) ;
#1591 = CARTESIAN_POINT ( 'NONE',  ( 2.449293598294706513E-15, -20.00000000000000000, 9.000000000000000000 ) ) ;
#1592 = AXIS2_PLACEMENT_3D ( 'NONE', #15790, #2371, #14304 ) ;
#1593 = CARTESIAN_POINT ( 'NONE',  ( 54.13287192849676188, 62.29948385550240886, 5.649768623646098220 ) ) ;
#1594 = AXIS2_PLACEMENT_3D ( 'NONE', #7740, #4809, #4899 ) ;
#1595 = CARTESIAN_POINT ( 'NONE',  ( 4.000000000000000000, 2.309401076758497151, -3.433295621305379353 ) ) ;
#1596 = DIRECTION ( 'NONE',  ( 1.000000000000000000, 0.000000000000000000, 0.000000000000000000 ) ) ;
#1597 = DIRECTION ( 'NONE',  ( -0.000000000000000000, -0.000000000000000000, 1.000000000000000000 ) ) ;
#1598 = CARTESIAN_POINT ( 'NONE',  ( 55.96859303347804371, 60.19948385550240744, 4.306917132069425946 ) ) ;
#1599 = AXIS2_PLACEMENT_3D ( 'NONE', #1314, #2979, #19182 ) ;
#1600 = CARTESIAN_POINT ( 'NONE',  ( -18.89043790736547379, -17.90943073464699609, 9.000000000000000000 ) ) ;
#1601 = CARTESIAN_POINT ( 'NONE',  ( 56.81924384183011512, 56.19948385550240744, 4.924951120819313743 ) ) ;
#1602 = FACE_BOUND ( 'NONE', #7020, .T. ) ;
#1603 = ADVANCED_FACE ( 'NONE', ( #8937 ), #14920, .F. ) ;
#1604 = CARTESIAN_POINT ( 'NONE',  ( 56.66441430157294690, 52.90051614449765793, -2.141517661632166281 ) ) ;
#1605 = DIRECTION ( 'NONE',  ( 0.000000000000000000, 0.000000000000000000, 1.000000000000000000 ) ) ;
#1606 = EDGE_CURVE ( 'NONE', #15143, #8758, #16211, .T. ) ;
#1607 = AXIS2_PLACEMENT_3D ( 'NONE', #1997, #7773, #4752 ) ;
#1608 = ORIENTED_EDGE ( 'NONE', *, *, #6329, .F. ) ;
#1609 = PRESENTATION_STYLE_ASSIGNMENT (( #17632 ) ) ;
#1610 = CIRCLE ( 'NONE', #3790, 0.9999999999999993339 ) ;
#1611 = ORIENTED_EDGE ( 'NONE', *, *, #14954, .T. ) ;
#1612 = CIRCLE ( 'NONE', #10047, 0.9999999999999997780 ) ;
#1613 = ADVANCED_FACE ( 'NONE', ( #13831 ), #12652, .F. ) ;
#1614 = EDGE_CURVE ( 'NONE', #10922, #10528, #6471, .T. ) ;
#1615 = LINE ( 'NONE', #4924, #2513 ) ;
#1616 = VERTEX_POINT ( 'NONE', #12557 ) ;
#1617 = DIRECTION ( 'NONE',  ( 0.000000000000000000, 0.000000000000000000, -1.000000000000000000 ) ) ;
#1618 = ADVANCED_FACE ( 'NONE', ( #9596, #12451, #10883 ), #2072, .F. ) ;
#1619 = CARTESIAN_POINT ( 'NONE',  ( 49.97728705011488159, 65.49948385550240459, -7.000000000000000888 ) ) ;
#1620 = EDGE_CURVE ( 'NONE', #6069, #8597, #7945, .T. ) ;
#1621 = CARTESIAN_POINT ( 'NONE',  ( -62.49999999999997158, 20.00000000000001421, -15.00000000000000000 ) ) ;
#1622 = ORIENTED_EDGE ( 'NONE', *, *, #2088, .F. ) ;
#1623 = FACE_OUTER_BOUND ( 'NONE', #18650, .T. ) ;
#1624 = DIRECTION ( 'NONE',  ( -1.000000000000000000, -0.000000000000000000, -0.000000000000000000 ) ) ;
#1625 = CARTESIAN_POINT ( 'NONE',  ( 49.97728705011488870, 57.49948385550241170, -6.000000000000000888 ) ) ;
#1626 = DIRECTION ( 'NONE',  ( 1.000000000000000000, 0.000000000000000000, 0.000000000000000000 ) ) ;
#1627 = CARTESIAN_POINT ( 'NONE',  ( 0.1996310553826630974, 1.947030205581109730, -5.000000000000000888 ) ) ;
#1628 = AXIS2_PLACEMENT_3D ( 'NONE', #3357, #15497, #5009 ) ;
#1629 = CARTESIAN_POINT ( 'NONE',  ( 50.02271294988505446, 52.50051614449766646, -8.000000000000001776 ) ) ;
#1630 = EDGE_CURVE ( 'NONE', #13816, #11065, #19042, .T. ) ;
#1631 = CARTESIAN_POINT ( 'NONE',  ( 46.45491332379576477, 53.70051614449766220, 4.840751629271188961 ) ) ;
#1632 = AXIS2_PLACEMENT_3D ( 'NONE', #16940, #17303, #18232 ) ;
#1633 = EDGE_CURVE ( 'NONE', #2794, #3573, #8136, .T. ) ;
#1634 = CARTESIAN_POINT ( 'NONE',  ( 3.511755186886750923, -2.826662030176382956, -3.597382984111582083 ) ) ;
#1635 = DIRECTION ( 'NONE',  ( -0.000000000000000000, -0.000000000000000000, -1.000000000000000000 ) ) ;
#1636 = ORIENTED_EDGE ( 'NONE', *, *, #8355, .T. ) ;
#1637 = ORIENTED_EDGE ( 'NONE', *, *, #8002, .F. ) ;
#1638 = CARTESIAN_POINT ( 'NONE',  ( 54.31203442848995877, 44.90264883920728778, -4.999999999999999112 ) ) ;
#1639 = ORIENTED_EDGE ( 'NONE', *, *, #8427, .F. ) ;
#1640 = EDGE_CURVE ( 'NONE', #7188, #13385, #11165, .T. ) ;
#1641 = CARTESIAN_POINT ( 'NONE',  ( 0.4465819873852039379, 5.773502691896261751, 3.331019006688249527E-17 ) ) ;
#1642 = DIRECTION ( 'NONE',  ( 0.000000000000000000, 1.000000000000000000, -1.073081856240829552E-16 ) ) ;
#1643 = VERTEX_POINT ( 'NONE', #4823 ) ;
#1644 = DIRECTION ( 'NONE',  ( -0.000000000000000000, -0.000000000000000000, -1.000000000000000000 ) ) ;
#1645 = CARTESIAN_POINT ( 'NONE',  ( 0.000000000000000000, 0.5192545390863916310, -1.000000000000000000 ) ) ;
#1646 = CIRCLE ( 'NONE', #5709, 20.00000000000000000 ) ;
#1647 = ORIENTED_EDGE ( 'NONE', *, *, #11926, .F. ) ;
#1648 = LINE ( 'NONE', #7515, #16648 ) ;
#1649 = VERTEX_POINT ( 'NONE', #1788 ) ;
#1650 = CARTESIAN_POINT ( 'NONE',  ( 43.20883090819745576, 48.79948385550240175, 4.963592699179006473 ) ) ;
#1651 = LINE ( 'NONE', #6240, #4142 ) ;
#1652 = CARTESIAN_POINT ( 'NONE',  ( 47.70284917648453415, 55.39948385550238896, -6.992620115222774047 ) ) ;
#1653 = PLANE ( 'NONE',  #14230 ) ;
#1654 = SURFACE_STYLE_USAGE ( .BOTH. , #1744 ) ;
#1655 = CARTESIAN_POINT ( 'NONE',  ( 52.25172492374527877, 55.40051614449764372, 7.007379884777203749 ) ) ;
#1656 = DIRECTION ( 'NONE',  ( -0.000000000000000000, -0.000000000000000000, 1.000000000000000000 ) ) ;
#1657 = CARTESIAN_POINT ( 'NONE',  ( -54.99999999999996447, -22.99999999999998579, -10.00000000000000000 ) ) ;
#1658 = AXIS2_PLACEMENT_3D ( 'NONE', #6218, #16429, #16626 ) ;
#1659 = CARTESIAN_POINT ( 'NONE',  ( -4.000000000000000000, 1.700094919196744270, -3.320312364301766017 ) ) ;
#1660 = ORIENTED_EDGE ( 'NONE', *, *, #12863, .F. ) ;
#1661 = ORIENTED_EDGE ( 'NONE', *, *, #11349, .F. ) ;
#1662 = ORIENTED_EDGE ( 'NONE', *, *, #635, .F. ) ;
#1663 = CARTESIAN_POINT ( 'NONE',  ( 73.00000000000000000, 3.000000000000000000, 6.000000000000000000 ) ) ;
#1664 = CARTESIAN_POINT ( 'NONE',  ( 47.70284917648453415, 47.39948385550238896, -6.992620115222774047 ) ) ;
#1665 = ORIENTED_EDGE ( 'NONE', *, *, #2942, .F. ) ;
#1666 = CARTESIAN_POINT ( 'NONE',  ( 6.420058897733093239, 5.782965130189194447, -1.451745169709246731E-16 ) ) ;
#1667 = ORIENTED_EDGE ( 'NONE', *, *, #4858, .F. ) ;
#1668 = CARTESIAN_POINT ( 'NONE',  ( 50.02271294988505446, 62.50051614449766646, -7.000000000000000888 ) ) ;
#1669 = ORIENTED_EDGE ( 'NONE', *, *, #7372, .T. ) ;
#1670 = EDGE_CURVE ( 'NONE', #17840, #7933, #3375, .T. ) ;
#1671 = CARTESIAN_POINT ( 'NONE',  ( 4.630153689607048761, 0.000000000000000000, -5.371010071662833063 ) ) ;
#1672 = UNCERTAINTY_MEASURE_WITH_UNIT (LENGTH_MEASURE( 1.000000000000000082E-05 ), #16777, 'distance_accuracy_value', 'NONE');
#1673 = LINE ( 'NONE', #1763, #11789 ) ;
#1674 = ORIENTED_EDGE ( 'NONE', *, *, #15749, .F. ) ;
#1675 = CARTESIAN_POINT ( 'NONE',  ( 48.07319477248762496, 52.40051614449767214, -6.007379884777208190 ) ) ;
#1676 = DIRECTION ( 'NONE',  ( 0.000000000000000000, 0.000000000000000000, -1.000000000000000000 ) ) ;
#1677 = EDGE_CURVE ( 'NONE', #12007, #15146, #3992, .T. ) ;
#1678 = DIRECTION ( 'NONE',  ( 1.000000000000000000, 0.000000000000000000, -0.000000000000000000 ) ) ;
#1679 = CARTESIAN_POINT ( 'NONE',  ( 44.28664221472220675, 59.09948385550240602, -1.832500667257165317 ) ) ;
#1680 = DIRECTION ( 'NONE',  ( 1.000000000000000000, -0.000000000000000000, 0.000000000000000000 ) ) ;
#1681 = CARTESIAN_POINT ( 'NONE',  ( 49.97728705011495265, 51.50051614449765935, 8.000000000000001776 ) ) ;
#1682 = DIRECTION ( 'NONE',  ( -0.000000000000000000, -0.000000000000000000, 1.000000000000000000 ) ) ;
#1683 = CARTESIAN_POINT ( 'NONE',  ( 4.052424581287787042, 2.393186648133419414, -2.990837702970412959 ) ) ;
#1684 = ORIENTED_EDGE ( 'NONE', *, *, #3634, .F. ) ;
#1685 = DIRECTION ( 'NONE',  ( -1.000000000000000000, -0.000000000000000000, -0.000000000000000000 ) ) ;
#1686 = PRODUCT_CONTEXT ( 'NONE', #1394, 'mechanical' ) ;
#1687 = EDGE_LOOP ( 'NONE', ( #4671, #16930, #7091 ) ) ;
#1688 = CARTESIAN_POINT ( 'NONE',  ( 0.000000000000000000, -3.031088913245534755, -1.750000000000001332 ) ) ;
#1689 = CARTESIAN_POINT ( 'NONE',  ( 0.000000000000000000, 0.000000000000000000, 0.000000000000000000 ) ) ;
#1690 = CARTESIAN_POINT ( 'NONE',  ( 54.09612160359786515, 61.69948385550240744, -5.676469297603166098 ) ) ;
#1691 = DIRECTION ( 'NONE',  ( -0.000000000000000000, -0.000000000000000000, -1.000000000000000000 ) ) ;
#1692 = DIRECTION ( 'NONE',  ( 1.000000000000000000, 0.000000000000000000, -0.000000000000000000 ) ) ;
#1693 = CARTESIAN_POINT ( 'NONE',  ( 49.99999999999997158, 65.00000000000002842, -7.000000000000000888 ) ) ;
#1694 = CARTESIAN_POINT ( 'NONE',  ( 56.66441430157296821, 60.09948385550240602, 2.141517661632100111 ) ) ;
#1695 = LINE ( 'NONE', #13350, #15160 ) ;
#1696 = CARTESIAN_POINT ( 'NONE',  ( 45.31609314410967926, 52.69948385550240744, 6.485486291978119766 ) ) ;
#1697 = CARTESIAN_POINT ( 'NONE',  ( 4.086262629614029862, -1.979770830881092181, -3.570936333571104626 ) ) ;
#1698 = CARTESIAN_POINT ( 'NONE',  ( 43.34962307344078880, 52.10051614449766078, -2.184720259617096705 ) ) ;
#1699 = CARTESIAN_POINT ( 'NONE',  ( -150.9999999999999432, -14.99999999999999645, -15.79999999999999538 ) ) ;
#1700 = AXIS2_PLACEMENT_3D ( 'NONE', #15352, #5146, #453 ) ;
#1701 = PRESENTATION_STYLE_ASSIGNMENT (( #4745 ) ) ;
#1702 = ORIENTED_EDGE ( 'NONE', *, *, #16732, .F. ) ;
#1703 = VECTOR ( 'NONE', #3262, 1000.000000000000000 ) ;
#1704 = CARTESIAN_POINT ( 'NONE',  ( 6.495567275915088423, 2.917443832164887230, -5.053160945538039961 ) ) ;
#1705 = ORIENTED_EDGE ( 'NONE', *, *, #3062, .F. ) ;
#1706 = CARTESIAN_POINT ( 'NONE',  ( 2.100000000000000089, 0.000000000000000000, -4.694516984716113228 ) ) ;
#1707 = EDGE_CURVE ( 'NONE', #3916, #848, #17010, .T. ) ;
#1708 = CARTESIAN_POINT ( 'NONE',  ( 49.97728705011488159, 63.49948385550241170, -7.000000000000000888 ) ) ;
#1709 = CYLINDRICAL_SURFACE ( 'NONE', #10850, 20.00000000000000000 ) ;
#1710 = ORIENTED_EDGE ( 'NONE', *, *, #14219, .F. ) ;
#1711 = DIRECTION ( 'NONE',  ( 0.000000000000000000, 0.000000000000000000, 1.000000000000000000 ) ) ;
#1712 = CARTESIAN_POINT ( 'NONE',  ( -154.9999999999999716, -14.99999999999999645, 15.00000000000000000 ) ) ;
#1713 = CARTESIAN_POINT ( 'NONE',  ( 44.28664221472220675, 55.09948385550241312, -1.832500667257165317 ) ) ;
#1714 = PLANE ( 'NONE',  #11650 ) ;
#1715 = CARTESIAN_POINT ( 'NONE',  ( 2.449293598294706513E-15, -20.00000000000000000, 9.000000000000000000 ) ) ;
#1716 = CARTESIAN_POINT ( 'NONE',  ( 58.41169779390614281, 55.00051614449766646, 0.02388180880515032231 ) ) ;
#1717 = CARTESIAN_POINT ( 'NONE',  ( 53.50833635130544508, 53.30051614449767072, 4.867452303228181343 ) ) ;
#1718 = LINE ( 'NONE', #5130, #3483 ) ;
#1719 = CARTESIAN_POINT ( 'NONE',  ( 6.507056315241516842, -5.826803161468474102, 0.09231912136634916333 ) ) ;
#1720 = ORIENTED_EDGE ( 'NONE', *, *, #9029, .T. ) ;
#1721 = ADVANCED_FACE ( 'NONE', ( #15306 ), #699, .F. ) ;
#1722 = ORIENTED_EDGE ( 'NONE', *, *, #10632, .F. ) ;
#1723 = CARTESIAN_POINT ( 'NONE',  ( 0.3126073911695746443, -2.020725942163797750, -3.499999999999999556 ) ) ;
#1724 = ORIENTED_EDGE ( 'NONE', *, *, #17366, .F. ) ;
#1725 = LINE ( 'NONE', #2186, #13300 ) ;
#1726 = DIRECTION ( 'NONE',  ( -0.000000000000000000, -0.000000000000000000, -1.000000000000000000 ) ) ;
#1727 = CIRCLE ( 'NONE', #3925, 20.00000000000000000 ) ;
#1728 = ORIENTED_EDGE ( 'NONE', *, *, #11541, .F. ) ;
#1729 = AXIS2_PLACEMENT_3D ( 'NONE', #5086, #9578, #3243 ) ;
#1730 = CARTESIAN_POINT ( 'NONE',  ( 2.449293598294706513E-15, -20.00000000000000000, 9.000000000000000000 ) ) ;
#1731 = EDGE_CURVE ( 'NONE', #10976, #5141, #9505, .T. ) ;
#1732 = CARTESIAN_POINT ( 'NONE',  ( 44.03140696652193498, 49.19948385550240744, -4.306917132069424170 ) ) ;
#1733 = EDGE_CURVE ( 'NONE', #4148, #11140, #595, .T. ) ;
#1734 = EDGE_CURVE ( 'NONE', #4109, #9092, #4630, .T. ) ;
#1735 = ORIENTED_EDGE ( 'NONE', *, *, #11053, .F. ) ;
#1736 = DIRECTION ( 'NONE',  ( -1.000000000000000000, 0.000000000000000000, 0.000000000000000000 ) ) ;
#1737 = ORIENTED_EDGE ( 'NONE', *, *, #9233, .F. ) ;
#1738 = CARTESIAN_POINT ( 'NONE',  ( 47.42335538002188144, 46.59948385550239891, 8.007379884777233059 ) ) ;
#1739 = CYLINDRICAL_SURFACE ( 'NONE', #17926, 12.49999999999999645 ) ;
#1740 =( GEOMETRIC_REPRESENTATION_CONTEXT ( 3 ) GLOBAL_UNCERTAINTY_ASSIGNED_CONTEXT ( ( #16964 ) ) GLOBAL_UNIT_ASSIGNED_CONTEXT ( ( #13852, #6690, #719 ) ) REPRESENTATION_CONTEXT ( 'NONE', 'WORKASPACE' ) );
#1741 = ADVANCED_FACE ( 'NONE', ( #1887 ), #7759, .T. ) ;
#1742 = CARTESIAN_POINT ( 'NONE',  ( 52.29715082351547295, 58.39948385550238896, 6.992620115222774047 ) ) ;
#1743 = CARTESIAN_POINT ( 'NONE',  ( 6.244297270355323448, 0.4917101305082447471, 5.105276777067912164 ) ) ;
#1744 = SURFACE_SIDE_STYLE ('',( #3024 ) ) ;
#1745 = CARTESIAN_POINT ( 'NONE',  ( 50.02271294988505446, 52.50051614449765935, -7.000000000000000888 ) ) ;
#1746 = ADVANCED_FACE ( 'NONE', ( #11559 ), #5589, .F. ) ;
#1747 = LINE ( 'NONE', #17038, #38 ) ;
#1748 = VERTEX_POINT ( 'NONE', #795 ) ;
#1749 = ORIENTED_EDGE ( 'NONE', *, *, #12259, .T. ) ;
#1750 = VERTEX_POINT ( 'NONE', #7058 ) ;
#1751 = CARTESIAN_POINT ( 'NONE',  ( -8.134732861515892921, -38.27090915285207018, -9.000000000000000000 ) ) ;
#1752 = CIRCLE ( 'NONE', #7684, 0.9999999999999985567 ) ;
#1753 = CARTESIAN_POINT ( 'NONE',  ( 49.97728705011486738, 65.49948385550240459, -8.000000000000001776 ) ) ;
#1754 = CARTESIAN_POINT ( 'NONE',  ( 17.32050807568887052, -29.99999999999984013, -9.000000000000000000 ) ) ;
#1755 = ORIENTED_EDGE ( 'NONE', *, *, #4727, .T. ) ;
#1756 = DIRECTION ( 'NONE',  ( 1.000000000000000000, 0.000000000000000000, 0.000000000000000000 ) ) ;
#1757 = ADVANCED_FACE ( 'NONE', ( #3837 ), #8625, .T. ) ;
#1758 = EDGE_CURVE ( 'NONE', #3235, #16171, #4029, .T. ) ;
#1759 = ORIENTED_EDGE ( 'NONE', *, *, #16169, .F. ) ;
#1760 = CARTESIAN_POINT ( 'NONE',  ( 47.74827507625470702, 60.40051614449766504, -7.007379884777204637 ) ) ;
#1761 = VERTEX_POINT ( 'NONE', #4126 ) ;
#1762 = DIRECTION ( 'NONE',  ( 0.02857142857142857401, -0.9995917534020515305, 0.000000000000000000 ) ) ;
#1763 = CARTESIAN_POINT ( 'NONE',  ( 30.00000000000000000, 3.000000000000000000, 6.000000000000000000 ) ) ;
#1764 = CARTESIAN_POINT ( 'NONE',  ( 51.92680522751238925, 57.40051614449767214, 6.007379884777208190 ) ) ;
#1765 = CARTESIAN_POINT ( 'NONE',  ( -2.649999999999989697, 15.00000000000001599, -9.000000000000001776 ) ) ;
#1766 = VECTOR ( 'NONE', #7150, 1000.000000000000000 ) ;
#1767 = CARTESIAN_POINT ( 'NONE',  ( -74.99999999999997158, -39.99999999999998579, 10.00000000000000000 ) ) ;
#1768 = CARTESIAN_POINT ( 'NONE',  ( 56.30877334542961421, 55.99948385550241170, -0.02388180880520959434 ) ) ;
#1769 = CARTESIAN_POINT ( 'NONE',  ( -1.249999999999997780, 5.021051876504148371E-16, 4.100000000000000533 ) ) ;
#1770 = CARTESIAN_POINT ( 'NONE',  ( 57.60143344285435774, 53.10051614449767499, 2.493737253992045044 ) ) ;
#1771 = PLANE ( 'NONE',  #2184 ) ;
#1772 = AXIS2_PLACEMENT_3D ( 'NONE', #9114, #19244, #8723 ) ;
#1773 = ORIENTED_EDGE ( 'NONE', *, *, #11781, .T. ) ;
#1774 = CARTESIAN_POINT ( 'NONE',  ( -14.86289650954790886, -6.617387872822862782, -9.000000000000000000 ) ) ;
#1775 = FACE_OUTER_BOUND ( 'NONE', #921, .T. ) ;
#1776 = SHAPE_DEFINITION_REPRESENTATION ( #8187, #11935 ) ;
#1777 = ORIENTED_EDGE ( 'NONE', *, *, #4947, .T. ) ;
#1778 = CIRCLE ( 'NONE', #15227, 2.649999999999985700 ) ;
#1779 = DIRECTION ( 'NONE',  ( 0.000000000000000000, 0.000000000000000000, -1.000000000000000000 ) ) ;
#1780 = EDGE_CURVE ( 'NONE', #9457, #2897, #16089, .T. ) ;
#1781 = CARTESIAN_POINT ( 'NONE',  ( 75.00000000000001421, -7.499999999999971578, -20.00000000000000000 ) ) ;
#1782 = EDGE_CURVE ( 'NONE', #13131, #7980, #7122, .T. ) ;
#1783 = EDGE_CURVE ( 'NONE', #9539, #14693, #1067, .T. ) ;
#1784 = LINE ( 'NONE', #18362, #7518 ) ;
#1785 = CARTESIAN_POINT ( 'NONE',  ( 4.630153689607048761, 0.000000000000000000, 0.000000000000000000 ) ) ;
#1786 = CARTESIAN_POINT ( 'NONE',  ( -74.99999999999997158, 2.999999999999999112, 5.999999999999998224 ) ) ;
#1787 = AXIS2_PLACEMENT_3D ( 'NONE', #1037, #18895, #5430 ) ;
#1788 = CARTESIAN_POINT ( 'NONE',  ( -4.999999999999998224, -20.00000000000000000, -8.999999999999998224 ) ) ;
#1789 = CARTESIAN_POINT ( 'NONE',  ( 54.13287192849676188, 60.29948385550240886, 5.649768623646098220 ) ) ;
#1790 = CARTESIAN_POINT ( 'NONE',  ( 2.449293598294706513E-15, -20.00000000000000000, -9.000000000000000000 ) ) ;
#1791 = AXIS2_PLACEMENT_3D ( 'NONE', #862, #14184, #3611 ) ;
#1792 = CARTESIAN_POINT ( 'NONE',  ( 52.62207051974839089, 60.39948385550241028, 7.992620115222770494 ) ) ;
#1793 = B_SPLINE_CURVE_WITH_KNOTS ( 'NONE', 3,
 ( #15572, #7735, #12336, #15380, #9389, #6174, #15188, #15284 ),
 .UNSPECIFIED., .F., .F.,
 ( 4, 2, 2, 4 ),
 ( 0.002921158011986723767, 0.003648658599403076588, 0.004376159186819428976, 0.005831160361652133750 ),
 .UNSPECIFIED. ) ;
#1794 = CARTESIAN_POINT ( 'NONE',  ( 54.13287192849671214, 56.70051614449766220, -5.649768623646139964 ) ) ;
#1795 = DIRECTION ( 'NONE',  ( 1.000000000000000000, 0.000000000000000000, 0.000000000000000000 ) ) ;
#1796 = DIRECTION ( 'NONE',  ( -0.000000000000000000, -0.000000000000000000, 1.000000000000000000 ) ) ;
#1797 = ADVANCED_FACE ( 'NONE', ( #8328 ), #14308, .F. ) ;
#1798 = AXIS2_PLACEMENT_3D ( 'NONE', #18363, #8031, #10881 ) ;
#1799 = ORIENTED_EDGE ( 'NONE', *, *, #4544, .F. ) ;
#1800 = EDGE_CURVE ( 'NONE', #15771, #11016, #9606, .T. ) ;
#1801 = CIRCLE ( 'NONE', #19045, 15.00000000000000000 ) ;
#1802 = DIRECTION ( 'NONE',  ( 1.000000000000000000, 0.000000000000000000, 0.000000000000000000 ) ) ;
#1803 = CARTESIAN_POINT ( 'NONE',  ( 57.36023556966787851, 47.00051614449765935, 0.02388180880515038476 ) ) ;
#1804 = CARTESIAN_POINT ( 'NONE',  ( -179.9999999999999716, -15.00000000000000000, -9.000000000000000000 ) ) ;
#1805 = CARTESIAN_POINT ( 'NONE',  ( 1.398397006336996817, -6.091550361990593743, -0.8000000000000000444 ) ) ;
#1806 = VERTEX_POINT ( 'NONE', #8533 ) ;
#1807 = LINE ( 'NONE', #16713, #1159 ) ;
#1808 = LINE ( 'NONE', #7493, #11376 ) ;
#1809 = CARTESIAN_POINT ( 'NONE',  ( 53.54508667620424234, 44.70051614449765509, -4.840751629271188961 ) ) ;
#1810 = CARTESIAN_POINT ( 'NONE',  ( 50.00000000000000000, 15.00000000000000000, 4.000000000000003553 ) ) ;
#1811 =( NAMED_UNIT ( * ) PLANE_ANGLE_UNIT ( ) SI_UNIT ( $, .RADIAN. ) );
#1812 = CARTESIAN_POINT ( 'NONE',  ( 45.31609314410960820, 50.30051614449766362, -6.485486291978072693 ) ) ;
#1813 = CARTESIAN_POINT ( 'NONE',  ( 43.69122665457040000, 56.00051614449765935, -0.02388180880515696977 ) ) ;
#1814 = AXIS2_PLACEMENT_3D ( 'NONE', #15108, #6091, #12061 ) ;
#1815 = CARTESIAN_POINT ( 'NONE',  ( 0.3461262719736147297, -4.658553426539303821, -3.671615880910379381 ) ) ;
#1816 = VECTOR ( 'NONE', #550, 1000.000000000000000 ) ;
#1817 = DIRECTION ( 'NONE',  ( 0.000000000000000000, 0.000000000000000000, -1.000000000000000000 ) ) ;
#1818 = EDGE_LOOP ( 'NONE', ( #3421, #16160, #16447, #11886 ) ) ;
#1819 = ORIENTED_EDGE ( 'NONE', *, *, #10875, .T. ) ;
#1820 = DIRECTION ( 'NONE',  ( 1.000000000000000000, 0.000000000000000000, 0.000000000000000000 ) ) ;
#1821 = ORIENTED_EDGE ( 'NONE', *, *, #8177, .F. ) ;
#1822 = LINE ( 'NONE', #7693, #18162 ) ;
#1823 = AXIS2_PLACEMENT_3D ( 'NONE', #2602, #8645, #14618 ) ;
#1824 = ORIENTED_EDGE ( 'NONE', *, *, #9609, .T. ) ;
#1825 = CARTESIAN_POINT ( 'NONE',  ( 62.49999999999998579, 45.00000000000001421, -9.999999999999998224 ) ) ;
#1826 = CARTESIAN_POINT ( 'NONE',  ( 54.09612160359786515, 49.69948385550240744, -5.676469297603166098 ) ) ;
#1827 = AXIS2_PLACEMENT_3D ( 'NONE', #10171, #6070, #13414 ) ;
#1828 = ORIENTED_EDGE ( 'NONE', *, *, #5909, .F. ) ;
#1829 = DIRECTION ( 'NONE',  ( -0.000000000000000000, -0.000000000000000000, 1.000000000000000000 ) ) ;
#1830 = ORIENTED_EDGE ( 'NONE', *, *, #9857, .F. ) ;
#1831 = CARTESIAN_POINT ( 'NONE',  ( 43.18075615816994173, 63.80051614449766362, 4.924951120819380357 ) ) ;
#1832 = CARTESIAN_POINT ( 'NONE',  ( 3.349226789952652439, 2.685125164760731487, -0.2236248678334773199 ) ) ;
#1833 = CARTESIAN_POINT ( 'NONE',  ( 56.65037692655918988, 63.89948385550239607, -2.184720259617163762 ) ) ;
#1834 = DIRECTION ( 'NONE',  ( 0.000000000000000000, 0.000000000000000000, 1.000000000000000000 ) ) ;
#1835 =( LENGTH_UNIT ( ) NAMED_UNIT ( * ) SI_UNIT ( .MILLI., .METRE. ) );
#1836 = CARTESIAN_POINT ( 'NONE',  ( 44.05948171654945611, 52.20051614449764799, -4.345558710429044069 ) ) ;
#1837 = DIRECTION ( 'NONE',  ( 0.000000000000000000, 0.000000000000000000, 1.000000000000000000 ) ) ;
#1838 = CARTESIAN_POINT ( 'NONE',  ( 55.94051828345050836, 51.79948385550240175, -4.345558710429104465 ) ) ;
#1839 = DIRECTION ( 'NONE',  ( 0.000000000000000000, -0.000000000000000000, 1.000000000000000000 ) ) ;
#1840=STYLED_ITEM('',(#19468),#14915);
#1841 = EDGE_CURVE ( 'NONE', #16171, #2874, #10835, .T. ) ;
#1842 = AXIS2_PLACEMENT_3D ( 'NONE', #12809, #8386, #5449 ) ;
#1843 = ORIENTED_EDGE ( 'NONE', *, *, #1783, .F. ) ;
#1844 = ORIENTED_EDGE ( 'NONE', *, *, #13469, .F. ) ;
#1845 = CARTESIAN_POINT ( 'NONE',  ( 0.000000000000000000, 6.123233995736766282E-16, -5.000000000000000000 ) ) ;
#1846 = EDGE_CURVE ( 'NONE', #18783, #9833, #1137, .T. ) ;
#1847 = EDGE_CURVE ( 'NONE', #17135, #14839, #3874, .T. ) ;
#1848 = CARTESIAN_POINT ( 'NONE',  ( 55.94051828345050836, 49.79948385550240175, -4.345558710429104465 ) ) ;
#1849 = CARTESIAN_POINT ( 'NONE',  ( 3.973110223767137850, 2.263269463293572928E-11, 3.565797985667434222 ) ) ;
#1850 = STYLED_ITEM ( 'NONE', ( #2135 ), #11045 ) ;
#1851 = ORIENTED_EDGE ( 'NONE', *, *, #2242, .T. ) ;
#1852 = DIRECTION ( 'NONE',  ( 0.000000000000000000, 0.000000000000000000, 1.000000000000000000 ) ) ;
#1853 = EDGE_CURVE ( 'NONE', #13632, #5656, #14274, .T. ) ;
#1854 = EDGE_CURVE ( 'NONE', #7017, #7129, #17757, .T. ) ;
#1855 = ORIENTED_EDGE ( 'NONE', *, *, #1562, .T. ) ;
#1856 = CARTESIAN_POINT ( 'NONE',  ( 56.66441430157294690, 58.90051614449766504, -2.141517661632166281 ) ) ;
#1857 = VERTEX_POINT ( 'NONE', #199 ) ;
#1858 = CIRCLE ( 'NONE', #4353, 0.9999999999999995559 ) ;
#1859 = CONICAL_SURFACE ( 'NONE', #1842, 1.535500000000000087, 1.047197551196590748 ) ;
#1860 = EDGE_CURVE ( 'NONE', #16340, #14634, #12716, .T. ) ;
#1861 = CARTESIAN_POINT ( 'NONE',  ( 75.00000000000001421, -7.499999999999971578, -20.00000000000000000 ) ) ;
#1862 = PRODUCT_DEFINITION_CONTEXT ( 'detailed design', #13036, 'design' ) ;
#1863 = DIRECTION ( 'NONE',  ( 0.000000000000000000, 0.000000000000000000, 1.000000000000000000 ) ) ;
#1864 = CARTESIAN_POINT ( 'NONE',  ( 44.28664221472221385, 55.90051614449766504, 1.832500667257213722 ) ) ;
#1865 = FACE_BOUND ( 'NONE', #3419, .T. ) ;
#1866 = CARTESIAN_POINT ( 'NONE',  ( -162.9999999999999716, -14.99999999999999645, -15.00000000000000000 ) ) ;
#1867 = CARTESIAN_POINT ( 'NONE',  ( 48.02776887271745210, 65.39948385550239607, -5.992620115222778487 ) ) ;
#1868 = CARTESIAN_POINT ( 'NONE',  ( 6.244004651191001898, 4.178905357954649347, -2.972460101650454156 ) ) ;
#1869 = EDGE_CURVE ( 'NONE', #17340, #19190, #16799, .T. ) ;
#1870 = CARTESIAN_POINT ( 'NONE',  ( 41.58830220609386430, 62.00051614449766646, -0.02388180880514929535 ) ) ;
#1871 = EDGE_CURVE ( 'NONE', #8171, #3999, #4270, .T. ) ;
#1872 = ORIENTED_EDGE ( 'NONE', *, *, #3635, .F. ) ;
#1873 = DIRECTION ( 'NONE',  ( -0.000000000000000000, -0.000000000000000000, -1.000000000000000000 ) ) ;
#1874 = AXIS2_PLACEMENT_3D ( 'NONE', #13952, #15437, #13862 ) ;
#1875 = ORIENTED_EDGE ( 'NONE', *, *, #10485, .T. ) ;
#1876 = AXIS2_PLACEMENT_3D ( 'NONE', #10314, #5518, #10685 ) ;
#1877 = CARTESIAN_POINT ( 'NONE',  ( 0.000000000000000000, 0.000000000000000000, 0.000000000000000000 ) ) ;
#1878 = APPLICATION_PROTOCOL_DEFINITION ( 'draft international standard', 'automotive_design', 1998, #9275 ) ;
#1879 = VERTEX_POINT ( 'NONE', #10385 ) ;
#1880 = CARTESIAN_POINT ( 'NONE',  ( -16.32050807568879236, -10.00000000000004263, -9.000000000000000000 ) ) ;
#1881 = CARTESIAN_POINT ( 'NONE',  ( 8.134732861515777458, -1.729090847147875198, 9.000000000000000000 ) ) ;
#1882 = VECTOR ( 'NONE', #5606, 1000.000000000000000 ) ;
#1883 = DIRECTION ( 'NONE',  ( -1.000000000000000000, -0.000000000000000000, -0.000000000000000000 ) ) ;
#1884 = CARTESIAN_POINT ( 'NONE',  ( 7.500000000000003553, -20.00000000000000000, -20.00000000000000000 ) ) ;
#1885 = AXIS2_PLACEMENT_3D ( 'NONE', #2595, #11864, #19063 ) ;
#1886 = CARTESIAN_POINT ( 'NONE',  ( -150.9999999999999432, -14.99999999999999645, 17.00000000000000000 ) ) ;
#1887 = FACE_OUTER_BOUND ( 'NONE', #7540, .T. ) ;
#1888 = CARTESIAN_POINT ( 'NONE',  ( 53.50833635130540955, 47.69948385550240744, -4.867452303228209765 ) ) ;
#1889 = CARTESIAN_POINT ( 'NONE',  ( 3.951447005078450037, -1.347150628109123893, 3.500000000000000888 ) ) ;
#1890 = CARTESIAN_POINT ( 'NONE',  ( 43.20883090819745576, 56.79948385550240175, 4.963592699179006473 ) ) ;
#1891 = CARTESIAN_POINT ( 'NONE',  ( 49.97728705011495265, 57.50051614449766646, 7.000000000000000888 ) ) ;
#1892 = VECTOR ( 'NONE', #8776, 1000.000000000000000 ) ;
#1893 = CARTESIAN_POINT ( 'NONE',  ( 1.000000000000000000, -5.408326913195983465, -0.8000000000000000444 ) ) ;
#1894 = DIRECTION ( 'NONE',  ( -1.387778780781445991E-14, 0.000000000000000000, -1.000000000000000000 ) ) ;
#1895 = PRESENTATION_STYLE_ASSIGNMENT (( #15317 ) ) ;
#1896 = ORIENTED_EDGE ( 'NONE', *, *, #7841, .F. ) ;
#1897 = VECTOR ( 'NONE', #5185, 1000.000000000000000 ) ;
#1898 = CARTESIAN_POINT ( 'NONE',  ( -4.999999999999998224, -20.00000000000000000, 9.000000000000000000 ) ) ;
#1899 = VECTOR ( 'NONE', #16556, 1000.000000000000000 ) ;
#1900 = CIRCLE ( 'NONE', #12847, 12.49999999999999645 ) ;
#1901 = CARTESIAN_POINT ( 'NONE',  ( 47.74827507625470702, 46.40051614449765083, -7.007379884777204637 ) ) ;
#1902 = CARTESIAN_POINT ( 'NONE',  ( -57.64999999999994884, -14.99999999999998579, -15.00000000000000000 ) ) ;
#1903 = AXIS2_PLACEMENT_3D ( 'NONE', #15026, #13166, #1605 ) ;
#1904 = CYLINDRICAL_SURFACE ( 'NONE', #12420, 1.000000000000000888 ) ;
#1905 = EDGE_LOOP ( 'NONE', ( #18790, #2116, #961, #19284, #17506, #19084, #2223, #5330, #6132, #3508 ) ) ;
#1906 = CARTESIAN_POINT ( 'NONE',  ( 4.158806965674310518, -4.075748668183988066, -0.05940377217583901054 ) ) ;
#1907 = DIRECTION ( 'NONE',  ( 0.000000000000000000, 1.000000000000000000, -8.673617379884036458E-16 ) ) ;
#1908 = EDGE_CURVE ( 'NONE', #2621, #7384, #4316, .T. ) ;
#1909 = CARTESIAN_POINT ( 'NONE',  ( 50.02271294988511841, 60.49948385550240459, 6.000000000000000888 ) ) ;
#1910 = FACE_OUTER_BOUND ( 'NONE', #18333, .T. ) ;
#1911 = SURFACE_SIDE_STYLE ('',( #7497 ) ) ;
#1912 = CARTESIAN_POINT ( 'NONE',  ( 41.58830220609386430, 58.00051614449765935, -0.02388180880514929535 ) ) ;
#1913 = CIRCLE ( 'NONE', #15365, 0.9999999999999980016 ) ;
#1914 = EDGE_CURVE ( 'NONE', #75, #14471, #5837, .T. ) ;
#1915 = CARTESIAN_POINT ( 'NONE',  ( 55.11794222512599362, 54.80051614449764941, -3.688883143319583446 ) ) ;
#1916 = CARTESIAN_POINT ( 'NONE',  ( 50.00000000000000000, 15.00000000000000000, -4.000000000000003553 ) ) ;
#1917 = CONICAL_SURFACE ( 'NONE', #13170, 1.610000000000000098, 0.7853981633974658205 ) ;
#1918 = CARTESIAN_POINT ( 'NONE',  ( 6.212068001623061164, -3.310128279683368202, -4.266689640017852447 ) ) ;
#1919 = AXIS2_PLACEMENT_3D ( 'NONE', #8871, #10142, #14853 ) ;
#1920 = VERTEX_POINT ( 'NONE', #13532 ) ;
#1921 = STYLED_ITEM ( 'NONE', ( #19161 ), #9419 ) ;
#1922 = EDGE_LOOP ( 'NONE', ( #15863, #11906, #16343, #18581 ) ) ;
#1923 = FACE_OUTER_BOUND ( 'NONE', #13422, .T. ) ;
#1924 = ORIENTED_EDGE ( 'NONE', *, *, #13332, .T. ) ;
#1925 = CARTESIAN_POINT ( 'NONE',  ( -4.999999999999998224, -20.00000000000000000, 15.00000000000000355 ) ) ;
#1926 = SHAPE_REPRESENTATION ( 'spring', ( #10359 ), #6832 ) ;
#1927 = ORIENTED_EDGE ( 'NONE', *, *, #10034, .T. ) ;
#1928 = DIRECTION ( 'NONE',  ( 1.000000000000000000, 0.000000000000000000, 0.000000000000000000 ) ) ;
#1929 = CARTESIAN_POINT ( 'NONE',  ( 55.96859303347805081, 52.19948385550240033, 4.306917132069425058 ) ) ;
#1930 = ORIENTED_EDGE ( 'NONE', *, *, #7858, .T. ) ;
#1931 = CARTESIAN_POINT ( 'NONE',  ( -59.84999999999998721, 32.50000000000001421, 15.00000000000000000 ) ) ;
#1932 = AXIS2_PLACEMENT_3D ( 'NONE', #7610, #4581, #163 ) ;
#1933 = ORIENTED_EDGE ( 'NONE', *, *, #17501, .F. ) ;
#1934 = CARTESIAN_POINT ( 'NONE',  ( 41.58830220609386430, 52.99948385550241170, 0.02388180880523263147 ) ) ;
#1935 = AXIS2_PLACEMENT_3D ( 'NONE', #996, #797, #8331 ) ;
#1936 = CARTESIAN_POINT ( 'NONE',  ( 3.878104551856474735, -0.7018542299754126912, -3.499999999999999556 ) ) ;
#1937 = CARTESIAN_POINT ( 'NONE',  ( 46.45491332379572924, 47.29948385550241596, -4.840751629271157874 ) ) ;
#1938 = MANIFOLD_SOLID_BREP ( 'Fillet1', #12741 ) ;
#1939 = CARTESIAN_POINT ( 'NONE',  ( 4.114405500665261783, 2.025575754679710627, -3.508400121684937645 ) ) ;
#1940=STYLED_ITEM('',(#19454),#2528);
#1941 = CARTESIAN_POINT ( 'NONE',  ( 4.000000000000000000, -1.560351142792952617, -0.2242961665059816367 ) ) ;
#1942 = CARTESIAN_POINT ( 'NONE',  ( 54.09612160359792199, 63.30051614449766362, 5.676469297603124353 ) ) ;
#1943 = LINE ( 'NONE', #6149, #12265 ) ;
#1944 = CARTESIAN_POINT ( 'NONE',  ( 49.97728705011488159, 53.49948385550240459, -7.000000000000000888 ) ) ;
#1945 = CARTESIAN_POINT ( 'NONE',  ( 8.500000000000000000, 5.773502691896261751, 0.000000000000000000 ) ) ;
#1946 = ORIENTED_EDGE ( 'NONE', *, *, #5411, .T. ) ;
#1947 = CARTESIAN_POINT ( 'NONE',  ( 0.000000000000000000, 0.000000000000000000, 0.000000000000000000 ) ) ;
#1948 = CARTESIAN_POINT ( 'NONE',  ( 56.65037692655918988, 49.89948385550240317, -2.184720259617163762 ) ) ;
#1949 = AXIS2_PLACEMENT_3D ( 'NONE', #3122, #18123, #7519 ) ;
#1950 = FILL_AREA_STYLE ('',( #15560 ) ) ;
#1951 = ORIENTED_EDGE ( 'NONE', *, *, #17793, .F. ) ;
#1952 = DIRECTION ( 'NONE',  ( -1.000000000000000000, -0.000000000000000000, -0.000000000000000000 ) ) ;
#1953 = ORIENTED_EDGE ( 'NONE', *, *, #18219, .T. ) ;
#1954 = LINE ( 'NONE', #15566, #5039 ) ;
#1955 = ORIENTED_EDGE ( 'NONE', *, *, #11365, .T. ) ;
#1956 = ADVANCED_FACE ( 'NONE', ( #7351 ), #17961, .F. ) ;
#1957 = DIRECTION ( 'NONE',  ( 1.000000000000000000, 0.000000000000000000, -0.000000000000000000 ) ) ;
#1958 = CARTESIAN_POINT ( 'NONE',  ( 4.630153689607048761, 0.000000000000000000, 0.000000000000000000 ) ) ;
#1959 = PRODUCT_RELATED_PRODUCT_CATEGORY ( 'part', '', ( #11473 ) ) ;
#1960 = CARTESIAN_POINT ( 'NONE',  ( 46.45491332379576477, 63.70051614449766930, 4.840751629271188961 ) ) ;
#1961 = CARTESIAN_POINT ( 'NONE',  ( -1.249999999999998002, 4.599999999999999645, 0.000000000000000000 ) ) ;
#1962 = DIRECTION ( 'NONE',  ( -0.1045284632676563297, 0.9945218953682731788, 0.000000000000000000 ) ) ;
#1963 = CARTESIAN_POINT ( 'NONE',  ( -1.249999999999997558, 5.633375276077824112E-16, 4.599999999999999645 ) ) ;
#1964 = CARTESIAN_POINT ( 'NONE',  ( 50.02271294988505446, 58.50051614449765225, -8.000000000000001776 ) ) ;
#1965 = ORIENTED_EDGE ( 'NONE', *, *, #19295, .F. ) ;
#1966 = ORIENTED_EDGE ( 'NONE', *, *, #13563, .F. ) ;
#1967 = CARTESIAN_POINT ( 'NONE',  ( 0.1973348417602470706, -1.936114729415141733, 4.999999999999999112 ) ) ;
#1968 = ORIENTED_EDGE ( 'NONE', *, *, #15149, .F. ) ;
#1969 = DIRECTION ( 'NONE',  ( 0.000000000000000000, 0.000000000000000000, -1.000000000000000000 ) ) ;
#1970 = EDGE_CURVE ( 'NONE', #17741, #6607, #4613, .T. ) ;
#1971 = AXIS2_PLACEMENT_3D ( 'NONE', #5961, #1834, #12217 ) ;
#1972 = ORIENTED_EDGE ( 'NONE', *, *, #14831, .T. ) ;
#1973 = CARTESIAN_POINT ( 'NONE',  ( -17.32050807568872841, -30.00000000000008171, 9.000000000000000000 ) ) ;
#1974 = CARTESIAN_POINT ( 'NONE',  ( -29.99999999999999645, 0.000000000000000000, -10.00000000000000000 ) ) ;
#1975 = PRODUCT_DEFINITION_FORMATION_WITH_SPECIFIED_SOURCE ( 'ANY', '', #10075, .NOT_KNOWN. ) ;
#1976 = EDGE_CURVE ( 'NONE', #1616, #7030, #14586, .T. ) ;
#1977 = DIRECTION ( 'NONE',  ( -0.8090169943749487835, 0.5877852522924713607, 0.000000000000000000 ) ) ;
#1978 = EDGE_CURVE ( 'NONE', #18325, #2436, #4519, .T. ) ;
#1979 = CARTESIAN_POINT ( 'NONE',  ( 75.00000000000001421, -7.499999999999971578, -10.00000000000000000 ) ) ;
#1980 = FACE_OUTER_BOUND ( 'NONE', #5303, .T. ) ;
#1981 = DIRECTION ( 'NONE',  ( 0.000000000000000000, -1.000000000000000000, 8.673617379884035472E-16 ) ) ;
#1982 = CARTESIAN_POINT ( 'NONE',  ( 55.96859303347804371, 62.19948385550240744, 4.306917132069425946 ) ) ;
#1983 = CYLINDRICAL_SURFACE ( 'NONE', #3497, 5.000000000000000888 ) ;
#1984 = CARTESIAN_POINT ( 'NONE',  ( 50.02271294988513972, 62.49948385550240459, 8.000000000000001776 ) ) ;
#1985 = CARTESIAN_POINT ( 'NONE',  ( 54.13287192849671214, 60.70051614449766220, -5.649768623646139964 ) ) ;
#1986 = EDGE_CURVE ( 'NONE', #18910, #3513, #6765, .T. ) ;
#1987 = EDGE_CURVE ( 'NONE', #15553, #8337, #8329, .T. ) ;
#1988 = PRODUCT_DEFINITION_FORMATION_WITH_SPECIFIED_SOURCE ( 'ANY', '', #15860, .NOT_KNOWN. ) ;
#1989 = FACE_OUTER_BOUND ( 'NONE', #9536, .T. ) ;
#1990 = CARTESIAN_POINT ( 'NONE',  ( 6.244297270354683960, 1.802013835206515036E-11, 5.105276777067893512 ) ) ;
#1991 = EDGE_CURVE ( 'NONE', #5469, #3727, #10197, .T. ) ;
#1992 = B_SPLINE_CURVE_WITH_KNOTS ( 'NONE', 3,
 ( #8740, #11767, #16305, #14716, #14817 ),
 .UNSPECIFIED., .F., .F.,
 ( 4, 1, 4 ),
 ( 0.000000000000000000, 0.002886751345948130286, 0.005773502691896260572 ),
 .UNSPECIFIED. ) ;
#1993 = ORIENTED_EDGE ( 'NONE', *, *, #14194, .F. ) ;
#1994 = DIRECTION ( 'NONE',  ( -1.000000000000000000, 0.000000000000000000, 0.000000000000000000 ) ) ;
#1995 = CARTESIAN_POINT ( 'NONE',  ( 55.94051828345054389, 45.20051614449765509, 4.345558710429044957 ) ) ;
#1996 = B_SPLINE_CURVE_WITH_KNOTS ( 'NONE', 3,
 ( #14008, #4820, #5004, #15304, #15400 ),
 .UNSPECIFIED., .F., .F.,
 ( 4, 1, 4 ),
 ( 0.000000000000000000, 0.002020725942163690940, 0.004041451884327382747 ),
 .UNSPECIFIED. ) ;
#1997 = CARTESIAN_POINT ( 'NONE',  ( -154.9999999999999716, -14.99999999999999645, -9.000000000000000000 ) ) ;
#1998 = DIRECTION ( 'NONE',  ( 0.9135454576426060846, -0.4067366430757887730, 0.000000000000000000 ) ) ;
#1999 = ORIENTED_EDGE ( 'NONE', *, *, #3181, .F. ) ;
#2000 = DIRECTION ( 'NONE',  ( 0.000000000000000000, -1.000000000000000000, 0.000000000000000000 ) ) ;
#2001 = DIRECTION ( 'NONE',  ( -1.000000000000000000, -0.000000000000000000, -0.000000000000000000 ) ) ;
#2002 = CARTESIAN_POINT ( 'NONE',  ( 55.08986747509847248, 61.79948385550240175, -3.727524721679197572 ) ) ;
#2003 = CARTESIAN_POINT ( 'NONE',  ( -54.99999999999996447, -22.99999999999998579, 10.00000000000000000 ) ) ;
#2004 = CARTESIAN_POINT ( 'NONE',  ( 52.29715082351547295, 46.39948385550240317, 6.992620115222774047 ) ) ;
#2005 = DIRECTION ( 'NONE',  ( -0.000000000000000000, -0.000000000000000000, 1.000000000000000000 ) ) ;
#2006 = CARTESIAN_POINT ( 'NONE',  ( 47.42335538002180328, 60.40051614449765793, -8.007379884777206414 ) ) ;
#2007 = CARTESIAN_POINT ( 'NONE',  ( 44.91013252490150620, 60.20051614449766220, -3.727524721679154940 ) ) ;
#2008 = AXIS2_PLACEMENT_3D ( 'NONE', #3974, #14545, #4169 ) ;
#2009 = CYLINDRICAL_SURFACE ( 'NONE', #10982, 1.000000000000000000 ) ;
#2010 = VECTOR ( 'NONE', #1656, 1000.000000000000000 ) ;
#2011 = VERTEX_POINT ( 'NONE', #14697 ) ;
#2012 = EDGE_LOOP ( 'NONE', ( #9876, #7914, #1924, #13543 ) ) ;
#2013 = LINE ( 'NONE', #7788, #9049 ) ;
#2014 = ORIENTED_EDGE ( 'NONE', *, *, #18527, .F. ) ;
#2015 = EDGE_CURVE ( 'NONE', #8758, #2066, #17745, .T. ) ;
#2016 = LINE ( 'NONE', #10822, #5296 ) ;
#2017 = ORIENTED_EDGE ( 'NONE', *, *, #16957, .T. ) ;
#2018 = CARTESIAN_POINT ( 'NONE',  ( 0.000000000000000000, 0.000000000000000000, -4.000000000000000000 ) ) ;
#2019 = EDGE_CURVE ( 'NONE', #10823, #19206, #6361, .T. ) ;
#2020 = CARTESIAN_POINT ( 'NONE',  ( 56.65037692655918988, 53.89948385550240317, -2.184720259617163762 ) ) ;
#2021 = AXIS2_PLACEMENT_3D ( 'NONE', #12770, #10013, #11384 ) ;
#2022 = ORIENTED_EDGE ( 'NONE', *, *, #11676, .F. ) ;
#2023 = LINE ( 'NONE', #449, #17601 ) ;
#2024 = ORIENTED_EDGE ( 'NONE', *, *, #11567, .F. ) ;
#2025 =( REPRESENTATION_RELATIONSHIP ('NONE','NONE', #16703, #1297 ) REPRESENTATION_RELATIONSHIP_WITH_TRANSFORMATION ( #8317 )SHAPE_REPRESENTATION_RELATIONSHIP( ) );
#2026 = CARTESIAN_POINT ( 'NONE',  ( 45.31609314410967926, 50.69948385550240744, 6.485486291978119766 ) ) ;
#2027 = AXIS2_PLACEMENT_3D ( 'NONE', #17172, #6855, #12746 ) ;
#2028 = CARTESIAN_POINT ( 'NONE',  ( 0.000000000000000000, 20.00000000000001421, -9.999999999999998224 ) ) ;
#2029 = CARTESIAN_POINT ( 'NONE',  ( 54.13287192849676188, 64.29948385550241596, 5.649768623646098220 ) ) ;
#2030 = MANIFOLD_SOLID_BREP ( 'Cavity1', #16195 ) ;
#2031 = CARTESIAN_POINT ( 'NONE',  ( -72.99999999999997158, -1.000000000000000000, 6.000000000000001776 ) ) ;
#2032 = FACE_OUTER_BOUND ( 'NONE', #18602, .T. ) ;
#2033 = CARTESIAN_POINT ( 'NONE',  ( 43.34962307344078880, 58.10051614449766078, -2.184720259617096705 ) ) ;
#2034 = DIRECTION ( 'NONE',  ( -0.8090169943749487835, 0.5877852522924713607, 0.000000000000000000 ) ) ;
#2035 = CARTESIAN_POINT ( 'NONE',  ( 47.74827507625478518, 60.59948385550239891, 7.007379884777227730 ) ) ;
#2036 = LINE ( 'NONE', #1945, #10351 ) ;
#2037 = ORIENTED_EDGE ( 'NONE', *, *, #13822, .F. ) ;
#2038 = EDGE_LOOP ( 'NONE', ( #8946, #15241, #19336, #1559 ) ) ;
#2039 = LINE ( 'NONE', #18425, #5584 ) ;
#2040 = AXIS2_PLACEMENT_3D ( 'NONE', #6761, #14306, #8822 ) ;
#2041 = CARTESIAN_POINT ( 'NONE',  ( 57.36023556966787851, 49.99948385550238328, -0.02388180880522424582 ) ) ;
#2042 = CYLINDRICAL_SURFACE ( 'NONE', #285, 2.649999999999988365 ) ;
#2043 = EDGE_LOOP ( 'NONE', ( #9607, #6346 ) ) ;
#2044 = ORIENTED_EDGE ( 'NONE', *, *, #12883, .F. ) ;
#2045 = CARTESIAN_POINT ( 'NONE',  ( -154.8605857259444463, -18.79744172571344762, 15.79999999999999893 ) ) ;
#2046 = AXIS2_PLACEMENT_3D ( 'NONE', #16246, #19409, #10633 ) ;
#2047 = EDGE_LOOP ( 'NONE', ( #613, #18279, #8119, #17452 ) ) ;
#2048 = CARTESIAN_POINT ( 'NONE',  ( 55.94051828345054389, 63.20051614449764799, 4.345558710429044957 ) ) ;
#2049 = EDGE_LOOP ( 'NONE', ( #1684, #9569, #5626, #12124, #5368, #18796, #18625, #17262 ) ) ;
#2050 = PRODUCT_DEFINITION_CONTEXT ( 'detailed design', #12402, 'design' ) ;
#2051 = DIRECTION ( 'NONE',  ( 0.000000000000000000, -0.000000000000000000, 1.000000000000000000 ) ) ;
#2052 = CARTESIAN_POINT ( 'NONE',  ( 51.97223112728249816, 62.60051614449765367, -5.992620115222793586 ) ) ;
#2053 = CARTESIAN_POINT ( 'NONE',  ( -155.0777214229742071, -18.79920509849242549, 15.79999999999999893 ) ) ;
#2054 = DIRECTION ( 'NONE',  ( -1.000000000000000000, -0.000000000000000000, -0.000000000000000000 ) ) ;
#2055 = CARTESIAN_POINT ( 'NONE',  ( 2.449293598294706513E-15, -20.00000000000000000, 9.000000000000000000 ) ) ;
#2056 = CIRCLE ( 'NONE', #18350, 4.799999999999999822 ) ;
#2057 = CARTESIAN_POINT ( 'NONE',  ( 52.62207051974829852, 58.60051614449766788, -7.992620115222797139 ) ) ;
#2058 = ORIENTED_EDGE ( 'NONE', *, *, #12323, .F. ) ;
#2059 = ORIENTED_EDGE ( 'NONE', *, *, #953, .F. ) ;
#2060 = DIRECTION ( 'NONE',  ( 0.6691306063588571273, 0.7431448254773952433, 0.000000000000000000 ) ) ;
#2061 = VECTOR ( 'NONE', #2153, 1000.000000000000000 ) ;
#2062 = DIRECTION ( 'NONE',  ( 0.000000000000000000, 0.000000000000000000, -1.000000000000000000 ) ) ;
#2063 = ORIENTED_EDGE ( 'NONE', *, *, #7478, .F. ) ;
#2064 = CARTESIAN_POINT ( 'NONE',  ( -154.9999999999999716, -14.99999999999999645, 10.00000000000000000 ) ) ;
#2065 = DIRECTION ( 'NONE',  ( 0.000000000000000000, 0.000000000000000000, -1.000000000000000000 ) ) ;
#2066 = VERTEX_POINT ( 'NONE', #16678 ) ;
#2067 = AXIS2_PLACEMENT_3D ( 'NONE', #11136, #18334, #7818 ) ;
#2068 = DIRECTION ( 'NONE',  ( 0.000000000000000000, 0.000000000000000000, -1.000000000000000000 ) ) ;
#2069 = UNCERTAINTY_MEASURE_WITH_UNIT (LENGTH_MEASURE( 1.000000000000000082E-05 ), #15917, 'distance_accuracy_value', 'NONE');
#2070 = DIRECTION ( 'NONE',  ( -1.000000000000000000, -0.000000000000000000, -0.000000000000000000 ) ) ;
#2071 = LINE ( 'NONE', #16695, #13282 ) ;
#2072 = PLANE ( 'NONE',  #12758 ) ;
#2073 = VECTOR ( 'NONE', #6267, 1000.000000000000000 ) ;
#2074 = CARTESIAN_POINT ( 'NONE',  ( 43.34962307344081012, 64.89948385550239607, 2.184720259617164650 ) ) ;
#2075 = CARTESIAN_POINT ( 'NONE',  ( 2.449293598294706513E-15, -20.00000000000000000, 15.00000000000000355 ) ) ;
#2076 = CARTESIAN_POINT ( 'NONE',  ( 47.42335538002188144, 58.59948385550239891, 8.007379884777233059 ) ) ;
#2077 = CARTESIAN_POINT ( 'NONE',  ( 49.97728705011495265, 59.50051614449765935, 7.000000000000000888 ) ) ;
#2078 = B_SPLINE_CURVE_WITH_KNOTS ( 'NONE', 3,
 ( #11055, #3614, #395, #12339, #1868, #6269, #9580, #481 ),
 .UNSPECIFIED., .F., .F.,
 ( 4, 2, 2, 4 ),
 ( 0.000000000000000000, 0.001493104274552340587, 0.002986208549104681607, 0.005972417098209364950 ),
 .UNSPECIFIED. ) ;
#2079 = DIRECTION ( 'NONE',  ( -1.000000000000000000, 0.000000000000000000, 1.224646799147353207E-16 ) ) ;
#2080 = DIRECTION ( 'NONE',  ( 0.000000000000000000, 0.5000000000000009992, -0.8660254037844380415 ) ) ;
#2081 = EDGE_CURVE ( 'NONE', #8420, #10947, #6442, .T. ) ;
#2082 = ORIENTED_EDGE ( 'NONE', *, *, #11418, .F. ) ;
#2083 = PLANE ( 'NONE',  #14222 ) ;
#2084 = EDGE_CURVE ( 'NONE', #965, #1167, #16868, .T. ) ;
#2085 = DIRECTION ( 'NONE',  ( 0.000000000000000000, 0.000000000000000000, -1.000000000000000000 ) ) ;
#2086 = CARTESIAN_POINT ( 'NONE',  ( 0.000000000000000000, 0.000000000000000000, 0.000000000000000000 ) ) ;
#2087 = EDGE_CURVE ( 'NONE', #3513, #12235, #18251, .T. ) ;
#2088 = EDGE_CURVE ( 'NONE', #488, #16920, #678, .T. ) ;
#2089 = DIRECTION ( 'NONE',  ( 1.000000000000000000, 0.000000000000000000, 0.000000000000000000 ) ) ;
#2090 = DIRECTION ( 'NONE',  ( 1.000000000000000000, 0.000000000000000000, 0.000000000000000000 ) ) ;
#2091 = ORIENTED_EDGE ( 'NONE', *, *, #12568, .F. ) ;
#2092 = LINE ( 'NONE', #17194, #5521 ) ;
#2093 = VECTOR ( 'NONE', #10324, 1000.000000000000000 ) ;
#2094 = CARTESIAN_POINT ( 'NONE',  ( -52.34999999999998010, -14.99999999999998579, 15.00000000000000000 ) ) ;
#2095 = EDGE_CURVE ( 'NONE', #2791, #16221, #9204, .T. ) ;
#2096 = CARTESIAN_POINT ( 'NONE',  ( 55.11794222512601493, 64.19948385550240744, 3.688883143319541702 ) ) ;
#2097 = CARTESIAN_POINT ( 'NONE',  ( -0.9999999999999976685, -20.00000000000000000, 8.999999999999998224 ) ) ;
#2098 = CARTESIAN_POINT ( 'NONE',  ( 54.13287192849676188, 46.29948385550240886, 5.649768623646098220 ) ) ;
#2099 = DIRECTION ( 'NONE',  ( 1.000000000000000000, 0.000000000000000000, 0.000000000000000000 ) ) ;
#2100 = CARTESIAN_POINT ( 'NONE',  ( 42.39856655714564226, 60.10051614449766788, -2.493737253992044156 ) ) ;
#2101 = CARTESIAN_POINT ( 'NONE',  ( 44.88205777487401349, 63.80051614449766362, 3.688883143319584779 ) ) ;
#2102 = CLOSED_SHELL ( 'NONE', ( #4793, #63, #16827, #318, #6766, #9044, #8811, #10108, #5089, #5235, #9436, #64, #16364, #16884, #4440, #2460, #1016, #18165 ) ) ;
#2103 = LINE ( 'NONE', #15724, #17590 ) ;
#2104 = CARTESIAN_POINT ( 'NONE',  ( -54.99999999999996447, -14.99999999999998579, 10.00000000000000000 ) ) ;
#2106 = EDGE_LOOP ( 'NONE', ( #1339, #12159, #11336, #17606 ) ) ;
#2105 = EDGE_CURVE ( 'NONE', #6699, #606, #12533, .T. ) ;
#2107 = VECTOR ( 'NONE', #18285, 1000.000000000000000 ) ;
#2108 = EDGE_CURVE ( 'NONE', #14634, #8760, #16789, .T. ) ;
#2109 = ORIENTED_EDGE ( 'NONE', *, *, #6644, .T. ) ;
#2110 = LINE ( 'NONE', #14243, #4354 ) ;
#2111 = VERTEX_POINT ( 'NONE', #1767 ) ;
#2112 = DIRECTION ( 'NONE',  ( -0.000000000000000000, 1.000000000000000000, -0.000000000000000000 ) ) ;
#2113 = VERTEX_POINT ( 'NONE', #13896 ) ;
#2114 = DIRECTION ( 'NONE',  ( -9.710251638871371392E-17, -5.969973981896233748E-17, -1.000000000000000000 ) ) ;
#2115 = CARTESIAN_POINT ( 'NONE',  ( 43.33558569842703179, 51.09948385550240602, -2.141517661632099223 ) ) ;
#2116 = ORIENTED_EDGE ( 'NONE', *, *, #4651, .T. ) ;
#2117 = CYLINDRICAL_SURFACE ( 'NONE', #15082, 2.149999999999999023 ) ;
#2118 = ORIENTED_EDGE ( 'NONE', *, *, #18878, .F. ) ;
#2119 = CARTESIAN_POINT ( 'NONE',  ( 58.41169779390614281, 51.99948385550239749, -0.02388180880523160798 ) ) ;
#2120 = CARTESIAN_POINT ( 'NONE',  ( -11.75570504584937481, -36.18033988749900942, -9.000000000000000000 ) ) ;
#2121 = CIRCLE ( 'NONE', #8046, 2.649999999999985700 ) ;
#2122 = CARTESIAN_POINT ( 'NONE',  ( 57.36023556966787851, 63.99948385550241881, -0.02388180880522424582 ) ) ;
#2123 = CARTESIAN_POINT ( 'NONE',  ( 3.974175853610013132, 2.726149789692839054, 2.409821656223150033 ) ) ;
#2124 = CARTESIAN_POINT ( 'NONE',  ( 4.082498951862920222, -4.041451884327386779, 0.000000000000000000 ) ) ;
#2125 = CIRCLE ( 'NONE', #15895, 2.000000000000000000 ) ;
#2126 = CARTESIAN_POINT ( 'NONE',  ( 52.25172492374527877, 59.40051614449765083, 7.007379884777203749 ) ) ;
#2127 = CARTESIAN_POINT ( 'NONE',  ( 56.66441430157296821, 58.09948385550240602, 2.141517661632100111 ) ) ;
#2128 = DIRECTION ( 'NONE',  ( -1.000000000000000000, 0.000000000000000000, 0.000000000000000000 ) ) ;
#2129 = DIRECTION ( 'NONE',  ( -1.000000000000000000, -0.000000000000000000, -0.000000000000000000 ) ) ;
#2130 = VERTEX_POINT ( 'NONE', #6451 ) ;
#2131 = ADVANCED_FACE ( 'NONE', ( #3523 ), #16968, .F. ) ;
#2132 = CIRCLE ( 'NONE', #10569, 0.4999999999999972244 ) ;
#2133 = ORIENTED_EDGE ( 'NONE', *, *, #13598, .F. ) ;
#2134 = FACE_OUTER_BOUND ( 'NONE', #12540, .T. ) ;
#2135 = PRESENTATION_STYLE_ASSIGNMENT (( #15555 ) ) ;
#2136 = VECTOR ( 'NONE', #2285, 1000.000000000000000 ) ;
#2137 = EDGE_CURVE ( 'NONE', #3410, #5817, #10817, .T. ) ;
#2138 = CARTESIAN_POINT ( 'NONE',  ( 54.09612160359786515, 53.69948385550240744, -5.676469297603166098 ) ) ;
#2139 =( NAMED_UNIT ( * ) PLANE_ANGLE_UNIT ( ) SI_UNIT ( $, .RADIAN. ) );
#2140 = ORIENTED_EDGE ( 'NONE', *, *, #5820, .F. ) ;
#2141 = ORIENTED_EDGE ( 'NONE', *, *, #15552, .F. ) ;
#2142 = DIRECTION ( 'NONE',  ( 0.000000000000000000, 0.000000000000000000, 1.000000000000000000 ) ) ;
#2143 = ORIENTED_EDGE ( 'NONE', *, *, #17441, .F. ) ;
#2144 = PRESENTATION_LAYER_ASSIGNMENT (  '', '', ( #14012 ) ) ;
#2145 = CARTESIAN_POINT ( 'NONE',  ( 4.000000000000001776, 2.694222958124178486E-16, 2.200000000000001066 ) ) ;
#2146 = ORIENTED_EDGE ( 'NONE', *, *, #16593, .T. ) ;
#2147 = CARTESIAN_POINT ( 'NONE',  ( 49.97728705011488159, 47.49948385550240459, -7.000000000000000888 ) ) ;
#2148 = LINE ( 'NONE', #3813, #18089 ) ;
#2149 = CARTESIAN_POINT ( 'NONE',  ( 48.02776887271750184, 59.60051614449765367, 5.992620115222795363 ) ) ;
#2150 = PLANE ( 'NONE',  #4228 ) ;
#2151 = VECTOR ( 'NONE', #2567, 1000.000000000000000 ) ;
#2152 = EDGE_CURVE ( 'NONE', #14471, #2159, #17422, .T. ) ;
#2153 = DIRECTION ( 'NONE',  ( -0.000000000000000000, -0.000000000000000000, 1.000000000000000000 ) ) ;
#2154 = DIRECTION ( 'NONE',  ( 1.000000000000000000, 0.000000000000000000, 0.000000000000000000 ) ) ;
#2155 = CARTESIAN_POINT ( 'NONE',  ( 42.38452918213190657, 59.90051614449767214, 2.450534656007115508 ) ) ;
#2156 = EDGE_CURVE ( 'NONE', #12421, #12768, #11090, .T. ) ;
#2157 =( GEOMETRIC_REPRESENTATION_CONTEXT ( 3 ) GLOBAL_UNCERTAINTY_ASSIGNED_CONTEXT ( ( #6171 ) ) GLOBAL_UNIT_ASSIGNED_CONTEXT ( ( #10942, #5159, #17043 ) ) REPRESENTATION_CONTEXT ( 'NONE', 'WORKASPACE' ) );
#2158 = ORIENTED_EDGE ( 'NONE', *, *, #1256, .F. ) ;
#2159 = VERTEX_POINT ( 'NONE', #9782 ) ;
#2160 = LINE ( 'NONE', #6554, #4949 ) ;
#2161 = CARTESIAN_POINT ( 'NONE',  ( 8.134732861516145164, -38.27090915285195649, 9.000000000000000000 ) ) ;
#2162 = ORIENTED_EDGE ( 'NONE', *, *, #1991, .T. ) ;
#2163 = CARTESIAN_POINT ( 'NONE',  ( 6.445379721942640749, -2.463581311471618740, -5.110653333236677476 ) ) ;
#2164 = COLOUR_RGB ( '',0.8941176470588234615, 0.8941176470588234615, 0.8941176470588234615 ) ;
#2165 = AXIS2_PLACEMENT_3D ( 'NONE', #6435, #13696, #16664 ) ;
#2166 = DIRECTION ( 'NONE',  ( -1.000000000000000000, 0.000000000000000000, 0.000000000000000000 ) ) ;
#2167 = ORIENTED_EDGE ( 'NONE', *, *, #12021, .F. ) ;
#2168 = B_SPLINE_CURVE_WITH_KNOTS ( 'NONE', 3,
 ( #13578, #1638, #16728, #7976, #6412, #16821 ),
 .UNSPECIFIED., .F., .F.,
 ( 4, 2, 4 ),
 ( 0.000000000000000000, 0.0003657767439067419277, 0.0007315534878134838555 ),
 .UNSPECIFIED. ) ;
#2169 = FACE_OUTER_BOUND ( 'NONE', #6068, .T. ) ;
#2170 = CARTESIAN_POINT ( 'NONE',  ( 15.00000000000000178, -20.00000000000000000, -50.00000000000000000 ) ) ;
#2171 =( GEOMETRIC_REPRESENTATION_CONTEXT ( 3 ) GLOBAL_UNCERTAINTY_ASSIGNED_CONTEXT ( ( #4414 ) ) GLOBAL_UNIT_ASSIGNED_CONTEXT ( ( #11985, #15951, #16609 ) ) REPRESENTATION_CONTEXT ( 'NONE', 'WORKASPACE' ) );
#2172 = DIRECTION ( 'NONE',  ( 1.000000000000000000, 0.000000000000000000, 0.000000000000000000 ) ) ;
#2173 = CARTESIAN_POINT ( 'NONE',  ( -154.9999999999999716, -14.99999999999999645, 9.000000000000000000 ) ) ;
#2174 = CARTESIAN_POINT ( 'NONE',  ( -2.449848172108560540, -3.432307619358754724, -3.503702292528910078 ) ) ;
#2175 = CARTESIAN_POINT ( 'NONE',  ( 51.92680522751233951, 45.59948385550240602, -6.007379884777223289 ) ) ;
#2176 = CARTESIAN_POINT ( 'NONE',  ( 2.449293598294706513E-15, -20.00000000000000000, 9.000000000000000000 ) ) ;
#2177 = CARTESIAN_POINT ( 'NONE',  ( 54.68390685589033495, 57.69948385550241454, -6.485486291978119766 ) ) ;
#2178 = CIRCLE ( 'NONE', #2497, 4.800000000000000711 ) ;
#2179 = CARTESIAN_POINT ( 'NONE',  ( 49.97728705011495265, 63.50051614449765935, 7.000000000000000888 ) ) ;
#2180 = AXIS2_PLACEMENT_3D ( 'NONE', #152, #15340, #15435 ) ;
#2181 = CARTESIAN_POINT ( 'NONE',  ( 5.000000000000003553, -20.00000000000000000, 15.00000000000000355 ) ) ;
#2182 = DIRECTION ( 'NONE',  ( -0.000000000000000000, -0.000000000000000000, -1.000000000000000000 ) ) ;
#2183 = DIRECTION ( 'NONE',  ( 0.000000000000000000, 0.000000000000000000, 1.000000000000000000 ) ) ;
#2184 = AXIS2_PLACEMENT_3D ( 'NONE', #13721, #6272, #18520 ) ;
#2185 = ORIENTED_EDGE ( 'NONE', *, *, #9202, .T. ) ;
#2186 = CARTESIAN_POINT ( 'NONE',  ( 0.9999999999999997780, -6.008326913195983998, -0.8000000000000000444 ) ) ;
#2187 = CARTESIAN_POINT ( 'NONE',  ( -65.14999999999996305, 32.50000000000001421, -10.00000000000000178 ) ) ;
#2188 = CARTESIAN_POINT ( 'NONE',  ( 56.65037692655921120, 53.10051614449766078, 2.184720259617097593 ) ) ;
#2189 = AXIS2_PLACEMENT_3D ( 'NONE', #14814, #14713, #1301 ) ;
#2190 = LINE ( 'NONE', #5406, #18794 ) ;
#2191 = DIRECTION ( 'NONE',  ( 0.5000000000000022204, 0.8660254037844374864, -0.000000000000000000 ) ) ;
#2192 = VERTEX_POINT ( 'NONE', #14487 ) ;
#2193 = DIRECTION ( 'NONE',  ( 0.000000000000000000, 0.000000000000000000, 1.000000000000000000 ) ) ;
#2194 = DIRECTION ( 'NONE',  ( -0.000000000000000000, -0.000000000000000000, 1.000000000000000000 ) ) ;
#2195 = EDGE_CURVE ( 'NONE', #7333, #6135, #9967, .T. ) ;
#2196 = DIRECTION ( 'NONE',  ( -0.000000000000000000, -0.000000000000000000, 1.000000000000000000 ) ) ;
#2197 = CARTESIAN_POINT ( 'NONE',  ( 55.96859303347804371, 48.19948385550240033, 4.306917132069425946 ) ) ;
#2198 = CIRCLE ( 'NONE', #5319, 20.00000000000000000 ) ;
#2199 = CARTESIAN_POINT ( 'NONE',  ( 2.449293598294706513E-15, -20.00000000000000000, -9.000000000000000000 ) ) ;
#2200 = CARTESIAN_POINT ( 'NONE',  ( 52.62207051974829852, 58.60051614449766788, -7.992620115222797139 ) ) ;
#2201 = EDGE_CURVE ( 'NONE', #439, #4800, #15844, .T. ) ;
#2202 = CARTESIAN_POINT ( 'NONE',  ( 43.69122665457040000, 62.00051614449766646, -0.02388180880515696977 ) ) ;
#2203 = DIRECTION ( 'NONE',  ( 0.000000000000000000, 0.000000000000000000, 1.000000000000000000 ) ) ;
#2204 = DIRECTION ( 'NONE',  ( 0.000000000000000000, -1.000000000000000000, 0.000000000000000000 ) ) ;
#2205 = AXIS2_PLACEMENT_3D ( 'NONE', #12647, #15591, #592 ) ;
#2206 = ORIENTED_EDGE ( 'NONE', *, *, #17255, .F. ) ;
#2207 = EDGE_CURVE ( 'NONE', #6347, #9398, #2557, .T. ) ;
#2208 = EDGE_CURVE ( 'NONE', #17459, #7605, #2451, .T. ) ;
#2209 = ORIENTED_EDGE ( 'NONE', *, *, #1620, .F. ) ;
#2210 = CIRCLE ( 'NONE', #9427, 3.799999999999999378 ) ;
#2211 = CIRCLE ( 'NONE', #10026, 8.099999999999999645 ) ;
#2212 = VERTEX_POINT ( 'NONE', #8306 ) ;
#2213 = DIRECTION ( 'NONE',  ( 0.000000000000000000, 0.000000000000000000, -1.000000000000000000 ) ) ;
#2214 = ORIENTED_EDGE ( 'NONE', *, *, #15651, .T. ) ;
#2215 = ADVANCED_FACE ( 'NONE', ( #7035 ), #14385, .T. ) ;
#2216 = CARTESIAN_POINT ( 'NONE',  ( -151.2002204621512078, -14.95906757097668027, -15.79999999999999893 ) ) ;
#2217 = EDGE_CURVE ( 'NONE', #62, #18826, #7388, .T. ) ;
#2218 = EDGE_LOOP ( 'NONE', ( #6703, #580, #17337, #12969, #17413, #15960, #6167, #14004, #1484, #17404, #17241, #18551 ) ) ;
#2219 = CARTESIAN_POINT ( 'NONE',  ( 2.449293598294706513E-15, -20.00000000000000000, 9.000000000000000000 ) ) ;
#2220 = CARTESIAN_POINT ( 'NONE',  ( 47.74827507625477807, 60.59948385550239891, 7.007379884777229506 ) ) ;
#2221 = EDGE_LOOP ( 'NONE', ( #8383, #13069, #10157, #7169 ) ) ;
#2222 = FACE_OUTER_BOUND ( 'NONE', #1276, .T. ) ;
#2223 = ORIENTED_EDGE ( 'NONE', *, *, #4224, .T. ) ;
#2224 = CARTESIAN_POINT ( 'NONE',  ( 57.61547081786812896, 54.09948385550241312, 2.450534656007040901 ) ) ;
#2225 = AXIS2_PLACEMENT_3D ( 'NONE', #14400, #14694, #5880 ) ;
#2226 = CARTESIAN_POINT ( 'NONE',  ( 5.686050877451574337, -5.768780236673276995, -1.000000000000000000 ) ) ;
#2227 = ADVANCED_FACE ( 'NONE', ( #18633 ), #18670, .F. ) ;
#2228 = CARTESIAN_POINT ( 'NONE',  ( 55.96859303347804371, 64.19948385550239323, 4.306917132069425946 ) ) ;
#2229 = CARTESIAN_POINT ( 'NONE',  ( 30.00000000000000355, 40.00000000000000000, 0.000000000000000000 ) ) ;
#2230 = ADVANCED_FACE ( 'NONE', ( #13018 ), #14284, .T. ) ;
#2231 = CARTESIAN_POINT ( 'NONE',  ( 4.175326769692858875, -4.121399112977860213, 3.677815466159040336E-14 ) ) ;
#2232 = CIRCLE ( 'NONE', #3769, 2.500000000000000888 ) ;
#2233 = CIRCLE ( 'NONE', #4098, 5.999999999999977796 ) ;
#2234 = CARTESIAN_POINT ( 'NONE',  ( 47.70284917648459100, 59.60051614449765367, 6.992620115222796251 ) ) ;
#2235 = CARTESIAN_POINT ( 'NONE',  ( 44.28664221472221385, 45.90051614449766504, 1.832500667257213722 ) ) ;
#2236 = AXIS2_PLACEMENT_3D ( 'NONE', #16897, #15123, #420 ) ;
#2237 = CARTESIAN_POINT ( 'NONE',  ( 47.74827507625478518, 58.59948385550238470, 7.007379884777227730 ) ) ;
#2238 = CARTESIAN_POINT ( 'NONE',  ( 6.466260427357672036, -2.904280683598005286, 5.030361703432631337 ) ) ;
#2239 = DIRECTION ( 'NONE',  ( 0.000000000000000000, 0.000000000000000000, 1.000000000000000000 ) ) ;
#2240 = ORIENTED_EDGE ( 'NONE', *, *, #11403, .T. ) ;
#2241 = ADVANCED_FACE ( 'NONE', ( #12828 ), #12923, .T. ) ;
#2242 = EDGE_CURVE ( 'NONE', #18552, #13579, #13641, .T. ) ;
#2243 = VERTEX_POINT ( 'NONE', #6942 ) ;
#2244 = FACE_OUTER_BOUND ( 'NONE', #4186, .T. ) ;
#2245 =( NAMED_UNIT ( * ) PLANE_ANGLE_UNIT ( ) SI_UNIT ( $, .RADIAN. ) );
#2246 = VECTOR ( 'NONE', #6356, 1000.000000000000000 ) ;
#2247 = EDGE_CURVE ( 'NONE', #6336, #11140, #18043, .T. ) ;
#2248 = CARTESIAN_POINT ( 'NONE',  ( 45.90387839640214196, 54.69948385550240744, 5.676469297603166098 ) ) ;
#2249 = DIRECTION ( 'NONE',  ( 0.000000000000000000, 0.000000000000000000, 1.000000000000000000 ) ) ;
#2250 = ORIENTED_EDGE ( 'NONE', *, *, #3903, .F. ) ;
#2251 = MECHANICAL_DESIGN_GEOMETRIC_PRESENTATION_REPRESENTATION (  '', ( #17791 ), #19282 ) ;
#2252 = ORIENTED_EDGE ( 'NONE', *, *, #11901, .T. ) ;
#2253 = DIRECTION ( 'NONE',  ( 2.191393683118470056E-17, 7.538405132783724027E-17, 1.000000000000000000 ) ) ;
#2254 = VERTEX_POINT ( 'NONE', #5566 ) ;
#2255 = DIRECTION ( 'NONE',  ( -0.000000000000000000, -0.000000000000000000, 1.000000000000000000 ) ) ;
#2256 = ORIENTED_EDGE ( 'NONE', *, *, #16352, .F. ) ;
#2257 = CARTESIAN_POINT ( 'NONE',  ( 54.09612160359786515, 47.69948385550240744, -5.676469297603166098 ) ) ;
#2258 = DIRECTION ( 'NONE',  ( -1.000000000000000000, -0.000000000000000000, -0.000000000000000000 ) ) ;
#2259 = CARTESIAN_POINT ( 'NONE',  ( 46.49166364869456913, 64.30051614449766362, -4.867452303228181343 ) ) ;
#2260 = CARTESIAN_POINT ( 'NONE',  ( 32.00000000000000000, 3.000000000000000000, -5.999999999999998224 ) ) ;
#2261 = DIRECTION ( 'NONE',  ( 0.000000000000000000, 0.000000000000000000, 1.000000000000000000 ) ) ;
#2262 = CARTESIAN_POINT ( 'NONE',  ( -54.99999999999996447, -14.99999999999998579, 10.00000000000000000 ) ) ;
#2263 = CIRCLE ( 'NONE', #1935, 2.500000000000000444 ) ;
#2264 = MANIFOLD_SOLID_BREP ( 'M5 Clearance Hole1', #17769 ) ;
#2265 = AXIS2_PLACEMENT_3D ( 'NONE', #10650, #9466, #13599 ) ;
#2266 = ORIENTED_EDGE ( 'NONE', *, *, #8508, .F. ) ;
#2267 = VERTEX_POINT ( 'NONE', #16264 ) ;
#2268 = PRESENTATION_STYLE_ASSIGNMENT (( #1076 ) ) ;
#2269 = ORIENTED_EDGE ( 'NONE', *, *, #3289, .T. ) ;
#2270 = CARTESIAN_POINT ( 'NONE',  ( -4.000000000000000888, -1.539600717839011201, -3.300726591567081591 ) ) ;
#2271 = ADVANCED_FACE ( 'NONE', ( #10165, #17256, #3027 ), #5965, .F. ) ;
#2272 = DIRECTION ( 'NONE',  ( -0.000000000000000000, -0.000000000000000000, -1.000000000000000000 ) ) ;
#2273 = ORIENTED_EDGE ( 'NONE', *, *, #14413, .F. ) ;
#2274 = EDGE_CURVE ( 'NONE', #5177, #8267, #5504, .T. ) ;
#2275 = DIRECTION ( 'NONE',  ( 1.000000000000000000, 0.000000000000000000, 0.000000000000000000 ) ) ;
#2276 = CARTESIAN_POINT ( 'NONE',  ( -4.141042297810615835, 2.227970268150415656, -3.687027686973619822 ) ) ;
#2277 = LINE ( 'NONE', #2574, #15817 ) ;
#2278 = CARTESIAN_POINT ( 'NONE',  ( 0.6666666666666658525, -4.233901974057276085, -3.300726591567086476 ) ) ;
#2279 = DIRECTION ( 'NONE',  ( 0.000000000000000000, 0.000000000000000000, 1.000000000000000000 ) ) ;
#2280 = CARTESIAN_POINT ( 'NONE',  ( 47.74827507625478518, 62.59948385550240602, 7.007379884777227730 ) ) ;
#2281 = DIRECTION ( 'NONE',  ( 0.000000000000000000, 0.000000000000000000, 1.000000000000000000 ) ) ;
#2282 = CARTESIAN_POINT ( 'NONE',  ( 42.39856655714566358, 64.89948385550239607, 2.493737253992119207 ) ) ;
#2283 = CARTESIAN_POINT ( 'NONE',  ( 44.05948171654945611, 64.20051614449765509, -4.345558710429044069 ) ) ;
#2284 = CIRCLE ( 'NONE', #8215, 2.149999999999999023 ) ;
#2285 = DIRECTION ( 'NONE',  ( -0.000000000000000000, -0.000000000000000000, -1.000000000000000000 ) ) ;
#2286 = CARTESIAN_POINT ( 'NONE',  ( 0.1713913650100259145, 0.000000000000000000, 0.000000000000000000 ) ) ;
#2287 = B_SPLINE_CURVE_WITH_KNOTS ( 'NONE', 3,
 ( #9702, #1889, #502, #7860, #414 ),
 .UNSPECIFIED., .F., .F.,
 ( 4, 1, 4 ),
 ( 0.000000000000000000, 0.002020725942163687470, 0.004041451884327374941 ),
 .UNSPECIFIED. ) ;
#2288 = CARTESIAN_POINT ( 'NONE',  ( 20.00000000000000000, -20.00000000000000000, -27.00000000000000355 ) ) ;
#2289 =( REPRESENTATION_RELATIONSHIP ('NONE','NONE', #16703, #10550 ) REPRESENTATION_RELATIONSHIP_WITH_TRANSFORMATION ( #15686 )SHAPE_REPRESENTATION_RELATIONSHIP( ) );
#2290 = ORIENTED_EDGE ( 'NONE', *, *, #1606, .T. ) ;
#2291 =( NAMED_UNIT ( * ) PLANE_ANGLE_UNIT ( ) SI_UNIT ( $, .RADIAN. ) );
#2292 = MANIFOLD_SOLID_BREP ( 'EndChamfer', #6791 ) ;
#2293 = CARTESIAN_POINT ( 'NONE',  ( 56.65037692655921120, 55.10051614449766078, 2.184720259617097593 ) ) ;
#2294 = CARTESIAN_POINT ( 'NONE',  ( 55.48859070151218020, 45.00000000000002132, -4.999999999999993783 ) ) ;
#2295 = CARTESIAN_POINT ( 'NONE',  ( 2.000000000000000000, 1.773042676681340524, -2.059984127722458425E-15 ) ) ;
#2296 = VERTEX_POINT ( 'NONE', #17836 ) ;
#2297 = FACE_OUTER_BOUND ( 'NONE', #18445, .T. ) ;
#2298 = CARTESIAN_POINT ( 'NONE',  ( -1.000000000000000000, -14.00000000000000000, -9.000000000000001776 ) ) ;
#2299 = DIRECTION ( 'NONE',  ( 0.3090169943749456194, 0.9510565162951541973, 0.000000000000000000 ) ) ;
#2300 = CARTESIAN_POINT ( 'NONE',  ( 52.29715082351547295, 48.39948385550240317, 6.992620115222774047 ) ) ;
#2301 = PRODUCT_DEFINITION_FORMATION_WITH_SPECIFIED_SOURCE ( 'ANY', '', #683, .NOT_KNOWN. ) ;
#2302 = CARTESIAN_POINT ( 'NONE',  ( -2.855764796983342624, 2.970025579236414082, -0.09382832055445475272 ) ) ;
#2303 = CARTESIAN_POINT ( 'NONE',  ( 54.68390685589033495, 47.69948385550240744, -6.485486291978119766 ) ) ;
#2304 = CARTESIAN_POINT ( 'NONE',  ( 53.54508667620424234, 62.70051614449766220, -4.840751629271188961 ) ) ;
#2305 = DIRECTION ( 'NONE',  ( 0.000000000000000000, -0.000000000000000000, 1.000000000000000000 ) ) ;
#2306 = DIRECTION ( 'NONE',  ( -0.000000000000000000, -1.000000000000000000, 8.673617379884035472E-16 ) ) ;
#2307 = EDGE_LOOP ( 'NONE', ( #16494, #1050, #12634, #12539 ) ) ;
#2308 = EDGE_LOOP ( 'NONE', ( #16052, #1529, #4400, #11353 ) ) ;
#2309 = ORIENTED_EDGE ( 'NONE', *, *, #9763, .F. ) ;
#2310 = DIRECTION ( 'NONE',  ( 0.000000000000000000, 0.000000000000000000, 1.000000000000000000 ) ) ;
#2311 = ORIENTED_EDGE ( 'NONE', *, *, #1970, .T. ) ;
#2312 = EDGE_CURVE ( 'NONE', #258, #18021, #11756, .T. ) ;
#2313 = DIRECTION ( 'NONE',  ( 0.000000000000000000, 8.673617379884036458E-16, 1.000000000000000000 ) ) ;
#2314 = ORIENTED_EDGE ( 'NONE', *, *, #7282, .F. ) ;
#2315 = DIRECTION ( 'NONE',  ( 0.000000000000000000, -1.000000000000000000, 8.673617379884035472E-16 ) ) ;
#2316 = CARTESIAN_POINT ( 'NONE',  ( 56.65037692655918988, 59.89948385550241028, -2.184720259617163762 ) ) ;
#2317 = ORIENTED_EDGE ( 'NONE', *, *, #16458, .T. ) ;
#2318 = CARTESIAN_POINT ( 'NONE',  ( 75.00000000000001421, 3.000000000000000888, 5.999999999999998224 ) ) ;
#2319 = EDGE_LOOP ( 'NONE', ( #2337, #1408, #3345, #11618 ) ) ;
#2320 = CARTESIAN_POINT ( 'NONE',  ( 45.31609314410967926, 52.69948385550240744, 6.485486291978119766 ) ) ;
#2321 = CARTESIAN_POINT ( 'NONE',  ( 4.000000000000000000, -2.309401076758516691, -0.4999999999999995559 ) ) ;
#2322 = CARTESIAN_POINT ( 'NONE',  ( 56.30877334542961421, 51.99948385550239749, -0.02388180880520959434 ) ) ;
#2323 = CIRCLE ( 'NONE', #2951, 20.00000000000000000 ) ;
#2324 = CARTESIAN_POINT ( 'NONE',  ( 3.958484000407329617, 3.734437307742037415, 0.5317648453100634054 ) ) ;
#2325 = CARTESIAN_POINT ( 'NONE',  ( -3.175194142252219631, -0.2536549670829674197, 9.000000000000000000 ) ) ;
#2326 = CARTESIAN_POINT ( 'NONE',  ( 54.09612160359792199, 61.30051614449766362, 5.676469297603124353 ) ) ;
#2327 = CIRCLE ( 'NONE', #4523, 24.99999999999999289 ) ;
#2328 = CARTESIAN_POINT ( 'NONE',  ( 51.92680522751233951, 63.59948385550239891, -6.007379884777223289 ) ) ;
#2329 = EDGE_CURVE ( 'NONE', #13768, #4796, #16555, .T. ) ;
#2330 = CARTESIAN_POINT ( 'NONE',  ( 44.05948171654949874, 58.79948385550240886, 4.345558710429105354 ) ) ;
#2331 = CARTESIAN_POINT ( 'NONE',  ( -1.240299975428134203E-15, -4.736529461165891242, -3.681130640444276292 ) ) ;
#2332 = CARTESIAN_POINT ( 'NONE',  ( 8.500000000000000000, -5.773502691896263528, 0.000000000000000000 ) ) ;
#2333 = ORIENTED_EDGE ( 'NONE', *, *, #7597, .T. ) ;
#2334 = ORIENTED_EDGE ( 'NONE', *, *, #17943, .F. ) ;
#2335 = FACE_OUTER_BOUND ( 'NONE', #7002, .T. ) ;
#2336 = FILL_AREA_STYLE_COLOUR ( '', #278 ) ;
#2337 = ORIENTED_EDGE ( 'NONE', *, *, #7587, .F. ) ;
#2338 = EDGE_CURVE ( 'NONE', #15553, #16440, #4198, .T. ) ;
#2339 = VECTOR ( 'NONE', #1907, 1000.000000000000000 ) ;
#2340 = CARTESIAN_POINT ( 'NONE',  ( 56.66441430157296821, 60.09948385550240602, 2.141517661632100111 ) ) ;
#2341 = EDGE_CURVE ( 'NONE', #1056, #14529, #13510, .T. ) ;
#2342 = DIRECTION ( 'NONE',  ( 0.000000000000000000, 0.000000000000000000, -1.000000000000000000 ) ) ;
#2343 = ORIENTED_EDGE ( 'NONE', *, *, #1860, .F. ) ;
#2344 = ORIENTED_EDGE ( 'NONE', *, *, #880, .T. ) ;
#2345 = VECTOR ( 'NONE', #15401, 1000.000000000000000 ) ;
#2346 = CYLINDRICAL_SURFACE ( 'NONE', #15218, 20.00000000000000000 ) ;
#2347 = ADVANCED_FACE ( 'NONE', ( #13305 ), #16353, .F. ) ;
#2348 = ORIENTED_EDGE ( 'NONE', *, *, #18323, .F. ) ;
#2349 = DIRECTION ( 'NONE',  ( 0.000000000000000000, 0.000000000000000000, 1.000000000000000000 ) ) ;
#2350 = ORIENTED_EDGE ( 'NONE', *, *, #15140, .F. ) ;
#2351 = EDGE_CURVE ( 'NONE', #1251, #11082, #4294, .T. ) ;
#2352 = CARTESIAN_POINT ( 'NONE',  ( 52.29715082351547295, 48.39948385550240317, 6.992620115222774047 ) ) ;
#2353 = CARTESIAN_POINT ( 'NONE',  ( 0.1217565302851100623, 3.710888496608919507, -0.5725525826504660465 ) ) ;
#2354 = CARTESIAN_POINT ( 'NONE',  ( 52.29715082351538769, 44.60051614449766788, -6.992620115222796251 ) ) ;
#2355 = CARTESIAN_POINT ( 'NONE',  ( 2.385244779468109755E-15, -20.00000000000000000, -9.999999999999994671 ) ) ;
#2356 = DIRECTION ( 'NONE',  ( 1.000000000000000000, 0.000000000000000000, 0.000000000000000000 ) ) ;
#2357 = MANIFOLD_SOLID_BREP ( 'FlangeHexFillet', #11799 ) ;
#2358 = ORIENTED_EDGE ( 'NONE', *, *, #6658, .T. ) ;
#2359 = ORIENTED_EDGE ( 'NONE', *, *, #16613, .F. ) ;
#2360 = CARTESIAN_POINT ( 'NONE',  ( 4.000000000000000000, -2.511475576507276042, -3.469253905236643565 ) ) ;
#2361 = EDGE_CURVE ( 'NONE', #10736, #18339, #18860, .T. ) ;
#2362 = DIRECTION ( 'NONE',  ( 1.000000000000000000, 0.000000000000000000, -0.000000000000000000 ) ) ;
#2363 = ADVANCED_FACE ( 'NONE', ( #3403 ), #4961, .T. ) ;
#2364 = CARTESIAN_POINT ( 'NONE',  ( -13.86289650954781649, -33.38261212717723936, -9.000000000000000000 ) ) ;
#2365 = CONTEXT_DEPENDENT_SHAPE_REPRESENTATION ( #13663, #19028 ) ;
#2366 = ORIENTED_EDGE ( 'NONE', *, *, #5865, .T. ) ;
#2367 = CARTESIAN_POINT ( 'NONE',  ( -11.75570504584948139, -3.819660112501066518, -9.000000000000000000 ) ) ;
#2368 = AXIS2_PLACEMENT_3D ( 'NONE', #697, #6958, #17567 ) ;
#2369 = VERTEX_POINT ( 'NONE', #18419 ) ;
#2370 = AXIS2_PLACEMENT_3D ( 'NONE', #8722, #12053, #16478 ) ;
#2371 = DIRECTION ( 'NONE',  ( -1.000000000000000000, -0.000000000000000000, -0.000000000000000000 ) ) ;
#2372 = FACE_OUTER_BOUND ( 'NONE', #14950, .T. ) ;
#2373 = CARTESIAN_POINT ( 'NONE',  ( 2.649999999999987477, 15.00000000000001599, 15.00000000000000178 ) ) ;
#2374 = VECTOR ( 'NONE', #11863, 1000.000000000000000 ) ;
#2375 = CARTESIAN_POINT ( 'NONE',  ( 4.170895651974848128, 2.054890354522668439, 3.559174498016340227 ) ) ;
#2376 = CARTESIAN_POINT ( 'NONE',  ( 44.88205777487398507, 53.19948385550240744, -3.688883143319540814 ) ) ;
#2377 = CARTESIAN_POINT ( 'NONE',  ( 10.00000000000000000, 15.00000000000001776, 15.00000000000000000 ) ) ;
#2378 = CARTESIAN_POINT ( 'NONE',  ( 52.25172492374522903, 45.59948385550240602, -7.007379884777225953 ) ) ;
#2379 = CARTESIAN_POINT ( 'NONE',  ( 44.05948171654945611, 62.20051614449764799, -4.345558710429044069 ) ) ;
#2380 = DIRECTION ( 'NONE',  ( -0.000000000000000000, 1.000000000000000000, 1.224646799147353207E-16 ) ) ;
#2381 = DIRECTION ( 'NONE',  ( -1.000000000000000000, 0.000000000000000000, 0.000000000000000000 ) ) ;
#2382 = EDGE_CURVE ( 'NONE', #15146, #12413, #6246, .T. ) ;
#2383 = DIRECTION ( 'NONE',  ( 0.000000000000000000, 0.000000000000000000, 1.000000000000000000 ) ) ;
#2384 = EDGE_CURVE ( 'NONE', #4462, #5527, #16668, .T. ) ;
#2385 = EDGE_LOOP ( 'NONE', ( #12298, #7289, #7016, #12127 ) ) ;
#2386 = LINE ( 'NONE', #8338, #14550 ) ;
#2387 = AXIS2_PLACEMENT_3D ( 'NONE', #17950, #10465, #3037 ) ;
#2388 = EDGE_CURVE ( 'NONE', #16919, #15771, #16974, .T. ) ;
#2389 = DIRECTION ( 'NONE',  ( 1.000000000000000000, 0.000000000000000000, 0.000000000000000000 ) ) ;
#2390 = CARTESIAN_POINT ( 'NONE',  ( 47.74827507625470702, 54.40051614449765793, -7.007379884777204637 ) ) ;
#2391 = CARTESIAN_POINT ( 'NONE',  ( -1.000000000000000000, -5.408326913195983465, -0.8000000000000000444 ) ) ;
#2392 = VECTOR ( 'NONE', #2054, 1000.000000000000000 ) ;
#2393 = CARTESIAN_POINT ( 'NONE',  ( 4.198928548860774157, -0.8158838809860124996, -3.526471437616918170 ) ) ;
#2394 = EDGE_LOOP ( 'NONE', ( #2109, #16729, #3489, #1178 ) ) ;
#2395 = CARTESIAN_POINT ( 'NONE',  ( -0.1374368770859596967, -4.808326913195983821, -0.8000000000000000444 ) ) ;
#2396 = DIRECTION ( 'NONE',  ( 0.000000000000000000, 0.4999999999999989453, -0.8660254037844391517 ) ) ;
#2397 = CARTESIAN_POINT ( 'NONE',  ( -74.99999999999997158, 40.00000000000001421, 10.00000000000000000 ) ) ;
#2398 = CARTESIAN_POINT ( 'NONE',  ( 54.09612160359786515, 49.69948385550240744, -5.676469297603166098 ) ) ;
#2399 = FACE_OUTER_BOUND ( 'NONE', #11479, .T. ) ;
#2400 = CARTESIAN_POINT ( 'NONE',  ( 50.02271294988513972, 48.49948385550241170, 8.000000000000001776 ) ) ;
#2401 = LINE ( 'NONE', #5416, #10995 ) ;
#2402 = AXIS2_PLACEMENT_3D ( 'NONE', #7221, #10062, #14374 ) ;
#2403 = CARTESIAN_POINT ( 'NONE',  ( 46.45491332379576477, 63.70051614449766930, 4.840751629271188961 ) ) ;
#2404 = EDGE_CURVE ( 'NONE', #17995, #15708, #18515, .T. ) ;
#2405 = DIRECTION ( 'NONE',  ( 1.000000000000000000, 0.000000000000000000, 0.000000000000000000 ) ) ;
#2406 = APPLICATION_CONTEXT ( 'automotive_design' ) ;
#2407 = CARTESIAN_POINT ( 'NONE',  ( 8.500000000000000000, 5.773502691896261751, -2.749426538070115714E-16 ) ) ;
#2408 = EDGE_LOOP ( 'NONE', ( #14780, #2520, #10341, #150 ) ) ;
#2409 = EDGE_CURVE ( 'NONE', #17731, #2854, #7621, .T. ) ;
#2410 = ORIENTED_EDGE ( 'NONE', *, *, #4119, .F. ) ;
#2411 = CARTESIAN_POINT ( 'NONE',  ( -154.8426517387881347, -18.99690399242885874, -15.79999999999999538 ) ) ;
#2412 = ORIENTED_EDGE ( 'NONE', *, *, #5447, .T. ) ;
#2413 = DIRECTION ( 'NONE',  ( 0.000000000000000000, -1.000000000000000000, 8.673617379884035472E-16 ) ) ;
#2414 = VECTOR ( 'NONE', #13659, 1000.000000000000000 ) ;
#2415 = ORIENTED_EDGE ( 'NONE', *, *, #3275, .T. ) ;
#2416 = CARTESIAN_POINT ( 'NONE',  ( 4.211140560182196957, 2.431303136016536470, -3.745885042887433514 ) ) ;
#2417 = CARTESIAN_POINT ( 'NONE',  ( 45.90387839640214196, 58.69948385550240033, 5.676469297603166098 ) ) ;
#2418 = ORIENTED_EDGE ( 'NONE', *, *, #18926, .T. ) ;
#2419 = FACE_OUTER_BOUND ( 'NONE', #859, .T. ) ;
#2420 = VERTEX_POINT ( 'NONE', #9185 ) ;
#2421 = CARTESIAN_POINT ( 'NONE',  ( 56.81924384183011512, 58.19948385550240744, 4.924951120819313743 ) ) ;
#2422 = DIRECTION ( 'NONE',  ( 0.000000000000000000, 0.000000000000000000, 1.000000000000000000 ) ) ;
#2423 = PRODUCT_DEFINITION_SHAPE ( 'NONE', 'NONE',  #19426 ) ;
#2424 = CARTESIAN_POINT ( 'NONE',  ( 44.28664221472220675, 53.09948385550240602, -1.832500667257165317 ) ) ;
#2425 = DIRECTION ( 'NONE',  ( -0.7071067811865533459, 8.659560562354861368E-17, -0.7071067811865416886 ) ) ;
#2426 = PLANE ( 'NONE',  #11494 ) ;
#2427 = CARTESIAN_POINT ( 'NONE',  ( 50.02271294988505446, 44.50051614449765935, -8.000000000000001776 ) ) ;
#2428 = CARTESIAN_POINT ( 'NONE',  ( 44.30067958973596376, 62.89948385550240317, 1.875703265242204099 ) ) ;
#2429 = CIRCLE ( 'NONE', #1478, 0.7500000000000000000 ) ;
#2430 = LINE ( 'NONE', #8381, #6912 ) ;
#2431 = VECTOR ( 'NONE', #5881, 1000.000000000000000 ) ;
#2432 = DIRECTION ( 'NONE',  ( -0.9999670257950099561, -0.008120795692649453515, 0.000000000000000000 ) ) ;
#2433 = VERTEX_POINT ( 'NONE', #3860 ) ;
#2434 = EDGE_LOOP ( 'NONE', ( #5923, #823, #6971, #7270 ) ) ;
#2435 = CARTESIAN_POINT ( 'NONE',  ( 0.4465819873849485311, -2.886751345948517677, -5.000000000000000000 ) ) ;
#2436 = VERTEX_POINT ( 'NONE', #1657 ) ;
#2437 = VECTOR ( 'NONE', #17878, 1000.000000000000000 ) ;
#2438 = CARTESIAN_POINT ( 'NONE',  ( 50.02271294988512551, 56.49948385550240459, 7.000000000000000888 ) ) ;
#2439 = FACE_OUTER_BOUND ( 'NONE', #7094, .T. ) ;
#2440 = ORIENTED_EDGE ( 'NONE', *, *, #14664, .T. ) ;
#2441 = ORIENTED_EDGE ( 'NONE', *, *, #8697, .T. ) ;
#2442 = DIRECTION ( 'NONE',  ( 1.000000000000000000, 0.000000000000000000, 0.000000000000000000 ) ) ;
#2443 = ORIENTED_EDGE ( 'NONE', *, *, #2361, .T. ) ;
#2444 = CARTESIAN_POINT ( 'NONE',  ( -30.00000000000000000, 3.000000000000000000, -5.999999999999994671 ) ) ;
#2445 = ORIENTED_EDGE ( 'NONE', *, *, #14107, .F. ) ;
#2446 = CARTESIAN_POINT ( 'NONE',  ( 56.65037692655918988, 53.89948385550240317, -2.184720259617163762 ) ) ;
#2447 = DIRECTION ( 'NONE',  ( 1.000000000000000000, 0.000000000000000000, 0.000000000000000000 ) ) ;
#2448 = CARTESIAN_POINT ( 'NONE',  ( 43.33558569842706021, 49.90051614449766504, 2.141517661632167169 ) ) ;
#2449 = LINE ( 'NONE', #8403, #3298 ) ;
#2450 = EDGE_CURVE ( 'NONE', #8156, #4950, #1943, .T. ) ;
#2451 = LINE ( 'NONE', #2653, #1449 ) ;
#2452 = DIRECTION ( 'NONE',  ( 0.000000000000000000, 0.000000000000000000, 1.000000000000000000 ) ) ;
#2453 = VECTOR ( 'NONE', #15403, 999.9999999999998863 ) ;
#2454 = EDGE_CURVE ( 'NONE', #2113, #6630, #5693, .T. ) ;
#2455 = EDGE_CURVE ( 'NONE', #1140, #4430, #17290, .T. ) ;
#2456 = CIRCLE ( 'NONE', #7754, 2.500000000000000444 ) ;
#2457 = ORIENTED_EDGE ( 'NONE', *, *, #3348, .T. ) ;
#2458 = EDGE_LOOP ( 'NONE', ( #13106, #3162, #17608 ) ) ;
#2459 = DIRECTION ( 'NONE',  ( -0.000000000000000000, -0.000000000000000000, 1.000000000000000000 ) ) ;
#2460 = ADVANCED_FACE ( 'NONE', ( #6430 ), #266, .F. ) ;
#2461 = EDGE_CURVE ( 'NONE', #17113, #11939, #8509, .T. ) ;
#2462 = DIRECTION ( 'NONE',  ( -2.191393683118470056E-17, -7.538405132783724027E-17, -1.000000000000000000 ) ) ;
#2463 = LINE ( 'NONE', #2364, #7777 ) ;
#2464 = EDGE_LOOP ( 'NONE', ( #7241, #7599, #2024 ) ) ;
#2465 = CARTESIAN_POINT ( 'NONE',  ( 0.000000000000000000, 0.000000000000000000, 0.000000000000000000 ) ) ;
#2466 = EDGE_CURVE ( 'NONE', #3507, #585, #4127, .T. ) ;
#2467 = VERTEX_POINT ( 'NONE', #18320 ) ;
#2468 = EDGE_LOOP ( 'NONE', ( #5928, #10210, #6351, #4158 ) ) ;
#2469 = VECTOR ( 'NONE', #4014, 1000.000000000000000 ) ;
#2470 = AXIS2_PLACEMENT_3D ( 'NONE', #16873, #4991, #3619 ) ;
#2471 = LINE ( 'NONE', #17464, #9096 ) ;
#2472 = DIRECTION ( 'NONE',  ( -1.000000000000000000, 0.000000000000000000, 0.000000000000000000 ) ) ;
#2473 = CARTESIAN_POINT ( 'NONE',  ( 44.30067958973596376, 64.89948385550239607, 1.875703265242204099 ) ) ;
#2474 = DIRECTION ( 'NONE',  ( -1.000000000000000000, 0.000000000000000000, 0.000000000000000000 ) ) ;
#2475 = EDGE_CURVE ( 'NONE', #2828, #10144, #6623, .T. ) ;
#2476 = CARTESIAN_POINT ( 'NONE',  ( 0.3126073911696408136, 2.020725942163688060, 3.500000000000000000 ) ) ;
#2477 = EDGE_CURVE ( 'NONE', #12254, #7385, #7260, .T. ) ;
#2478 = CARTESIAN_POINT ( 'NONE',  ( 55.69932041026404335, 51.89948385550241028, -1.875703265242203432 ) ) ;
#2479 = CARTESIAN_POINT ( 'NONE',  ( -3.175194142252219631, -0.2536549670829674197, -9.000000000000000000 ) ) ;
#2480 = CARTESIAN_POINT ( 'NONE',  ( 47.70284917648453415, 49.39948385550238896, -6.992620115222774047 ) ) ;
#2481 = CARTESIAN_POINT ( 'NONE',  ( 57.61547081786810764, 46.90051614449766504, -2.450534656007114176 ) ) ;
#2482 = DIRECTION ( 'NONE',  ( 0.000000000000000000, 0.000000000000000000, 1.000000000000000000 ) ) ;
#2483 = CARTESIAN_POINT ( 'NONE',  ( 2.449293598294706513E-15, -20.00000000000000000, -9.000000000000000000 ) ) ;
#2484 = CIRCLE ( 'NONE', #9348, 1.999999999999998224 ) ;
#2485 = CIRCLE ( 'NONE', #5285, 14.00000000000000000 ) ;
#2486 = SHAPE_REPRESENTATION_RELATIONSHIP ( 'NONE' , 'NONE' ,  #13919, #6604 ) ;
#2487 = VERTEX_POINT ( 'NONE', #553 ) ;
#2488 = DIRECTION ( 'NONE',  ( 1.000000000000000000, 0.000000000000000000, 0.000000000000000000 ) ) ;
#2489 = CARTESIAN_POINT ( 'NONE',  ( -74.99999999999997158, 40.00000000000001421, 10.00000000000000000 ) ) ;
#2490 = PRESENTATION_LAYER_ASSIGNMENT (  '', '', ( #9970 ) ) ;
#2491 = CARTESIAN_POINT ( 'NONE',  ( 45.90387839640208512, 54.30051614449765651, -5.676469297603124353 ) ) ;
#2492 = CARTESIAN_POINT ( 'NONE',  ( 0.000000000000000000, 0.4273491293402468805, -0.8000000000000000444 ) ) ;
#2493 = FACE_OUTER_BOUND ( 'NONE', #2738, .T. ) ;
#2494 = ORIENTED_EDGE ( 'NONE', *, *, #186, .T. ) ;
#2495 = CARTESIAN_POINT ( 'NONE',  ( 4.180231891692622881, -4.134807952925578789, -0.02076457676760693274 ) ) ;
#2496 = B_SPLINE_CURVE_WITH_KNOTS ( 'NONE', 3,
 ( #10548, #11730, #12027, #16261, #2744 ),
 .UNSPECIFIED., .F., .F.,
 ( 4, 1, 4 ),
 ( 0.000000000000000000, 0.002020725942163690506, 0.004041451884327381013 ),
 .UNSPECIFIED. ) ;
#2497 = AXIS2_PLACEMENT_3D ( 'NONE', #18498, #18305, #16731 ) ;
#2498 = CYLINDRICAL_SURFACE ( 'NONE', #6385, 8.000000000000007105 ) ;
#2499 = B_SPLINE_CURVE_WITH_KNOTS ( 'NONE', 3,
 ( #5193, #4026, #15791, #14204 ),
 .UNSPECIFIED., .F., .F.,
 ( 4, 4 ),
 ( 0.002977824986803859555, 0.005972417098209359745 ),
 .UNSPECIFIED. ) ;
#2500 = CARTESIAN_POINT ( 'NONE',  ( 3.540020015735602765, 2.810662092924382627, -3.602146406945867962 ) ) ;
#2501 = CARTESIAN_POINT ( 'NONE',  ( 43.33558569842703179, 53.09948385550240602, -2.141517661632099223 ) ) ;
#2502 = DIRECTION ( 'NONE',  ( 1.000000000000000000, 0.000000000000000000, -0.000000000000000000 ) ) ;
#2503 = CARTESIAN_POINT ( 'NONE',  ( 58.41169779390614281, 45.99948385550240459, -0.02388180880523160798 ) ) ;
#2504 = CARTESIAN_POINT ( 'NONE',  ( 0.1999999999999987899, 0.000000000000000000, 0.000000000000000000 ) ) ;
#2505 = CARTESIAN_POINT ( 'NONE',  ( 52.25172492374527877, 51.40051614449767214, 7.007379884777203749 ) ) ;
#2506 = MECHANICAL_DESIGN_GEOMETRIC_PRESENTATION_REPRESENTATION (  '', ( #15318 ), #3133 ) ;
#2507 = DIRECTION ( 'NONE',  ( 1.000000000000000000, 0.000000000000000000, 0.000000000000000000 ) ) ;
#2508 = DIRECTION ( 'NONE',  ( -1.000000000000000000, 0.000000000000000000, 0.000000000000000000 ) ) ;
#2509 = VERTEX_POINT ( 'NONE', #10839 ) ;
#2510 = VERTEX_POINT ( 'NONE', #16844 ) ;
#2511 = DIRECTION ( 'NONE',  ( 1.000000000000000000, -1.734723475976807341E-16, 0.000000000000000000 ) ) ;
#2512 = ORIENTED_EDGE ( 'NONE', *, *, #12998, .T. ) ;
#2513 = VECTOR ( 'NONE', #10893, 1000.000000000000000 ) ;
#2514 = AXIS2_PLACEMENT_3D ( 'NONE', #1877, #489, #1969 ) ;
#2515 = CARTESIAN_POINT ( 'NONE',  ( -4.000000000000000000, 0.3987449864459974846, -0.01220643443059782861 ) ) ;
#2516 = ORIENTED_EDGE ( 'NONE', *, *, #8072, .F. ) ;
#2517 = CARTESIAN_POINT ( 'NONE',  ( -1.000000000000000000, -14.00000000000000000, -9.000000000000001776 ) ) ;
#2518 = CARTESIAN_POINT ( 'NONE',  ( 54.09612160359786515, 57.69948385550240744, -5.676469297603166098 ) ) ;
#2519 = EDGE_CURVE ( 'NONE', #5544, #9930, #7883, .T. ) ;
#2520 = ORIENTED_EDGE ( 'NONE', *, *, #8892, .T. ) ;
#2521 = CIRCLE ( 'NONE', #19110, 0.5999999999999999778 ) ;
#2522 = CARTESIAN_POINT ( 'NONE',  ( 0.000000000000000000, 0.000000000000000000, -5.000000000000000000 ) ) ;
#2523 = VERTEX_POINT ( 'NONE', #11485 ) ;
#2524 = CARTESIAN_POINT ( 'NONE',  ( 45.31609314410967926, 60.69948385550240033, 6.485486291978119766 ) ) ;
#2525 = LINE ( 'NONE', #8374, #5767 ) ;
#2526 = EDGE_CURVE ( 'NONE', #5878, #8101, #2401, .T. ) ;
#2527 = CARTESIAN_POINT ( 'NONE',  ( 53.50833635130540955, 47.69948385550240744, -4.867452303228209765 ) ) ;
#2528 = MANIFOLD_SOLID_BREP ( 'Cavity1', #9591 ) ;
#2529 = CARTESIAN_POINT ( 'NONE',  ( 6.367873360227555679, -2.886751345948119774, 4.999999999999999112 ) ) ;
#2530 = FACE_OUTER_BOUND ( 'NONE', #13443, .T. ) ;
#2531 = CARTESIAN_POINT ( 'NONE',  ( 44.05948171654945611, 64.20051614449765509, -4.345558710429044069 ) ) ;
#2532 = CIRCLE ( 'NONE', #2845, 1.000000000000000000 ) ;
#2533 = CARTESIAN_POINT ( 'NONE',  ( 44.28664221472220675, 61.09948385550241312, -1.832500667257165317 ) ) ;
#2534 = DIRECTION ( 'NONE',  ( -0.000000000000000000, -0.000000000000000000, -1.000000000000000000 ) ) ;
#2535 = CARTESIAN_POINT ( 'NONE',  ( 0.000000000000000000, 0.000000000000000000, -0.8000000000000000444 ) ) ;
#2536 = ORIENTED_EDGE ( 'NONE', *, *, #9904, .F. ) ;
#2537 = CIRCLE ( 'NONE', #18184, 2.649999999999985700 ) ;
#2538 = VERTEX_POINT ( 'NONE', #14440 ) ;
#2539 = DIRECTION ( 'NONE',  ( -0.000000000000000000, -0.000000000000000000, 1.000000000000000000 ) ) ;
#2540 = ORIENTED_EDGE ( 'NONE', *, *, #11678, .T. ) ;
#2541 = CARTESIAN_POINT ( 'NONE',  ( 47.74827507625478518, 60.59948385550239891, 7.007379884777227730 ) ) ;
#2542 = DIRECTION ( 'NONE',  ( 0.000000000000000000, 0.000000000000000000, 1.000000000000000000 ) ) ;
#2543 = ORIENTED_EDGE ( 'NONE', *, *, #8682, .F. ) ;
#2544 = ORIENTED_EDGE ( 'NONE', *, *, #10861, .T. ) ;
#2545 = CARTESIAN_POINT ( 'NONE',  ( 2.449293598294706513E-15, -20.00000000000000000, 9.000000000000000000 ) ) ;
#2546 = AXIS2_PLACEMENT_3D ( 'NONE', #3628, #18454, #14567 ) ;
#2547 = ORIENTED_EDGE ( 'NONE', *, *, #17206, .F. ) ;
#2548 = CIRCLE ( 'NONE', #17575, 12.49999999999999645 ) ;
#2549 = CARTESIAN_POINT ( 'NONE',  ( 0.9996874511566102850, -0.02500000000000036915, 9.000000000000000000 ) ) ;
#2550 = AXIS2_PLACEMENT_3D ( 'NONE', #3299, #15637, #15439 ) ;
#2551 = ORIENTED_EDGE ( 'NONE', *, *, #9097, .T. ) ;
#2552 = CARTESIAN_POINT ( 'NONE',  ( 55.96859303347804371, 54.19948385550240033, 4.306917132069425946 ) ) ;
#2553 = LINE ( 'NONE', #14672, #17765 ) ;
#2554 = VECTOR ( 'NONE', #19275, 1000.000000000000114 ) ;
#2555 = CARTESIAN_POINT ( 'NONE',  ( 52.25172492374527877, 49.40051614449766504, 7.007379884777203749 ) ) ;
#2556 = FACE_OUTER_BOUND ( 'NONE', #16354, .T. ) ;
#2557 = LINE ( 'NONE', #14187, #8631 ) ;
#2558 = CARTESIAN_POINT ( 'NONE',  ( -154.9999999999999716, -14.99999999999999645, -15.00000000000000000 ) ) ;
#2559 = AXIS2_PLACEMENT_3D ( 'NONE', #1281, #8422, #19338 ) ;
#2560 = CIRCLE ( 'NONE', #6291, 20.00000000000000000 ) ;
#2561 = VERTEX_POINT ( 'NONE', #17689 ) ;
#2562 = ORIENTED_EDGE ( 'NONE', *, *, #10149, .F. ) ;
#2563 = CYLINDRICAL_SURFACE ( 'NONE', #3714, 20.00000000000000000 ) ;
#2564 =( LENGTH_UNIT ( ) NAMED_UNIT ( * ) SI_UNIT ( .MILLI., .METRE. ) );
#2565 = AXIS2_PLACEMENT_3D ( 'NONE', #6890, #2203, #2405 ) ;
#2566 = LINE ( 'NONE', #8524, #7436 ) ;
#2567 = DIRECTION ( 'NONE',  ( -0.000000000000000000, -0.000000000000000000, 1.000000000000000000 ) ) ;
#2568 = ORIENTED_EDGE ( 'NONE', *, *, #17667, .T. ) ;
#2569 = LINE ( 'NONE', #14496, #4883 ) ;
#2570 = ADVANCED_FACE ( 'NONE', ( #2695 ), #16027, .T. ) ;
#2571 = ORIENTED_EDGE ( 'NONE', *, *, #16055, .F. ) ;
#2572 = EDGE_LOOP ( 'NONE', ( #4284, #18886, #10853, #13287, #10251 ) ) ;
#2573 = DIRECTION ( 'NONE',  ( 1.000000000000000000, 0.000000000000000000, 0.000000000000000000 ) ) ;
#2574 = CARTESIAN_POINT ( 'NONE',  ( -74.99999999999997158, -1.000000000000000000, 6.000000000000001776 ) ) ;
#2575 = VECTOR ( 'NONE', #10158, 1000.000000000000000 ) ;
#2576 = CIRCLE ( 'NONE', #1628, 10.00000000000000888 ) ;
#2577 = CARTESIAN_POINT ( 'NONE',  ( 51.92680522751238925, 51.40051614449767214, 6.007379884777208190 ) ) ;
#2578 = DIRECTION ( 'NONE',  ( -0.000000000000000000, 0.000000000000000000, -1.000000000000000000 ) ) ;
#2579 = CARTESIAN_POINT ( 'NONE',  ( 4.114405500665256454, 2.025575754679711959, 3.508400121684935424 ) ) ;
#2580 = VECTOR ( 'NONE', #7710, 1000.000000000000000 ) ;
#2581 = CARTESIAN_POINT ( 'NONE',  ( 56.30877334542961421, 49.99948385550240459, -0.02388180880520959434 ) ) ;
#2582 = DIRECTION ( 'NONE',  ( 1.000000000000000000, 0.000000000000000000, 0.000000000000000000 ) ) ;
#2583 = CARTESIAN_POINT ( 'NONE',  ( 49.97728705011488159, 45.49948385550240459, -7.000000000000000888 ) ) ;
#2584 = CARTESIAN_POINT ( 'NONE',  ( 58.41169779390614281, 45.00051614449765225, 0.02388180880515032231 ) ) ;
#2585 = CARTESIAN_POINT ( 'NONE',  ( 9.037824375505676855, -37.84146099840244659, 0.000000000000000000 ) ) ;
#2586 = EDGE_CURVE ( 'NONE', #189, #17705, #1111, .T. ) ;
#2587 = LINE ( 'NONE', #14415, #2136 ) ;
#2588 = CARTESIAN_POINT ( 'NONE',  ( 6.092449800118089343, 3.827241605637482724, -3.371023086194387286 ) ) ;
#2589 = DIRECTION ( 'NONE',  ( 1.000000000000000000, 0.000000000000000000, 0.000000000000000000 ) ) ;
#2590 = EDGE_LOOP ( 'NONE', ( #2562, #12083, #16218, #3655 ) ) ;
#2591 = DIRECTION ( 'NONE',  ( -9.858538378746663627E-23, 5.031452844637890958E-23, -1.000000000000000000 ) ) ;
#2592 = EDGE_CURVE ( 'NONE', #3495, #7143, #10019, .T. ) ;
#2593 = PRODUCT_DEFINITION_SHAPE ( 'NONE', 'NONE',  #19431 ) ;
#2594 = ADVANCED_FACE ( 'NONE', ( #4243 ), #8649, .T. ) ;
#2595 = CARTESIAN_POINT ( 'NONE',  ( 1.267864665261691752E-11, -20.00000000000000000, 9.999999999999998224 ) ) ;
#2596 = CARTESIAN_POINT ( 'NONE',  ( 57.36023556966787851, 55.00051614449765935, 0.02388180880515038476 ) ) ;
#2597 = CYLINDRICAL_SURFACE ( 'NONE', #14386, 4.000000000000003553 ) ;
#2598 = CARTESIAN_POINT ( 'NONE',  ( 55.48859070151218020, 45.00000000000002132, -4.999999999999993783 ) ) ;
#2599 = EDGE_LOOP ( 'NONE', ( #3905, #17610, #16646, #4861 ) ) ;
#2600 = CARTESIAN_POINT ( 'NONE',  ( -158.7997795378487353, -15.04093242902330907, -15.79999999999999893 ) ) ;
#2601 = EDGE_CURVE ( 'NONE', #2467, #10823, #6887, .T. ) ;
#2602 = CARTESIAN_POINT ( 'NONE',  ( -54.99999999999996447, -14.99999999999998579, 10.00000000000000000 ) ) ;
#2603 = CARTESIAN_POINT ( 'NONE',  ( 52.25172492374522903, 53.59948385550241312, -7.007379884777225953 ) ) ;
#2604 = EDGE_CURVE ( 'NONE', #5450, #10423, #15096, .T. ) ;
#2605 = CARTESIAN_POINT ( 'NONE',  ( -54.99999999999996447, -14.99999999999998579, 10.00000000000000000 ) ) ;
#2606 = CARTESIAN_POINT ( 'NONE',  ( 45.31609314410960820, 64.30051614449766362, -6.485486291978072693 ) ) ;
#2607 = DIRECTION ( 'NONE',  ( 0.8571673013836855759, 1.049727191973305147E-16, -0.5150380737757258576 ) ) ;
#2608 = CARTESIAN_POINT ( 'NONE',  ( 57.36023556966787851, 47.00051614449764514, 0.02388180880515038476 ) ) ;
#2609 = EDGE_CURVE ( 'NONE', #16569, #8295, #8825, .T. ) ;
#2610 = CARTESIAN_POINT ( 'NONE',  ( 6.242789945155967857, 0.9948955795114693412, 5.105232858000414708 ) ) ;
#2611 = VERTEX_POINT ( 'NONE', #10119 ) ;
#2612 = ORIENTED_EDGE ( 'NONE', *, *, #1987, .T. ) ;
#2613 = DIRECTION ( 'NONE',  ( 0.000000000000000000, 0.000000000000000000, 1.000000000000000000 ) ) ;
#2614 = ORIENTED_EDGE ( 'NONE', *, *, #5937, .F. ) ;
#2615 = CARTESIAN_POINT ( 'NONE',  ( -17.79870116617248499, -10.87825472854618170, 9.000000000000000000 ) ) ;
#2616 = EDGE_LOOP ( 'NONE', ( #12882, #6834, #7414, #8836 ) ) ;
#2617 = DIRECTION ( 'NONE',  ( 1.000000000000000000, 0.000000000000000000, 0.000000000000000000 ) ) ;
#2618 = VERTEX_POINT ( 'NONE', #18972 ) ;
#2619 = DIRECTION ( 'NONE',  ( 0.000000000000000000, -0.000000000000000000, 1.000000000000000000 ) ) ;
#2620 = CARTESIAN_POINT ( 'NONE',  ( 75.00000000000000000, 32.50000000000001421, 15.00000000000000000 ) ) ;
#2621 = VERTEX_POINT ( 'NONE', #6983 ) ;
#2622 = CARTESIAN_POINT ( 'NONE',  ( 45.27934281921075410, 57.29948385550240175, -6.458785618021043895 ) ) ;
#2623 = B_SPLINE_CURVE_WITH_KNOTS ( 'NONE', 3,
 ( #6898, #11496, #2515, #18981, #5137, #17505, #11108, #17115 ),
 .UNSPECIFIED., .F., .F.,
 ( 4, 2, 2, 4 ),
 ( 0.005725059856848641743, 0.006314084072593626612, 0.006903108288338611481, 0.008081156719828581220 ),
 .UNSPECIFIED. ) ;
#2624 = CARTESIAN_POINT ( 'NONE',  ( 2.687328764639642653, -3.067272167851299969, -0.05923475698271395140 ) ) ;
#2625 = CARTESIAN_POINT ( 'NONE',  ( 44.88205777487398507, 51.19948385550240744, -3.688883143319540814 ) ) ;
#2626 = CARTESIAN_POINT ( 'NONE',  ( -57.64999999999994884, -14.99999999999998579, 15.00000000000000000 ) ) ;
#2627 = CARTESIAN_POINT ( 'NONE',  ( 3.129923130707922496, -23.63917314727666152, -8.999999999999996447 ) ) ;
#2628 = CARTESIAN_POINT ( 'NONE',  ( 56.81924384183006538, 48.80051614449767072, -4.924951120819380357 ) ) ;
#2629 = CARTESIAN_POINT ( 'NONE',  ( 44.30067958973594955, 48.10051614449766078, -1.875703265242155693 ) ) ;
#2630 = CARTESIAN_POINT ( 'NONE',  ( 4.630153689607048761, 0.000000000000000000, 0.000000000000000000 ) ) ;
#2631 = DIRECTION ( 'NONE',  ( 0.000000000000000000, 0.000000000000000000, 1.000000000000000000 ) ) ;
#2632 = ORIENTED_EDGE ( 'NONE', *, *, #9379, .F. ) ;
#2633 = ADVANCED_FACE ( 'NONE', ( #8354 ), #5512, .T. ) ;
#2634 = ORIENTED_EDGE ( 'NONE', *, *, #11770, .F. ) ;
#2635 = DIRECTION ( 'NONE',  ( -0.000000000000000000, -0.000000000000000000, -1.000000000000000000 ) ) ;
#2636 = SURFACE_SIDE_STYLE ('',( #15030 ) ) ;
#2637 = ORIENTED_EDGE ( 'NONE', *, *, #9615, .T. ) ;
#2638 = EDGE_CURVE ( 'NONE', #3507, #5600, #5380, .T. ) ;
#2639 = CARTESIAN_POINT ( 'NONE',  ( 57.36023556966787851, 57.99948385550239038, -0.02388180880522424582 ) ) ;
#2640 = PRESENTATION_STYLE_ASSIGNMENT (( #17531 ) ) ;
#2641 = ORIENTED_EDGE ( 'NONE', *, *, #5482, .F. ) ;
#2642 = ORIENTED_EDGE ( 'NONE', *, *, #118, .F. ) ;
#2643 = CARTESIAN_POINT ( 'NONE',  ( 2.000000000000000000, 1.329782007511004727, -0.7677500000000018199 ) ) ;
#2644 = DIRECTION ( 'NONE',  ( 0.000000000000000000, -1.224646799147353207E-16, 1.000000000000000000 ) ) ;
#2645 = ORIENTED_EDGE ( 'NONE', *, *, #17075, .T. ) ;
#2646 = CARTESIAN_POINT ( 'NONE',  ( -62.49999999999997158, 32.50000000000001421, 15.00000000000000000 ) ) ;
#2647 = VERTEX_POINT ( 'NONE', #33 ) ;
#2648 = FACE_OUTER_BOUND ( 'NONE', #9276, .T. ) ;
#2649 = CARTESIAN_POINT ( 'NONE',  ( 43.33558569842703179, 51.09948385550240602, -2.141517661632099223 ) ) ;
#2650 = CARTESIAN_POINT ( 'NONE',  ( 20.00000000000000000, -20.00000000000000000, -20.00000000000000000 ) ) ;
#2651 = CARTESIAN_POINT ( 'NONE',  ( 57.36023556966787851, 45.00051614449763804, 0.02388180880515038476 ) ) ;
#2652 = DIRECTION ( 'NONE',  ( -0.7779254092217071648, -0.6283566325640553840, 0.000000000000000000 ) ) ;
#2653 = CARTESIAN_POINT ( 'NONE',  ( -1.000000000000000000, -14.00000000000000000, 8.999999999999998224 ) ) ;
#2654 = LINE ( 'NONE', #15870, #13783 ) ;
#2655 = ADVANCED_FACE ( 'NONE', ( #10410 ), #4340, .F. ) ;
#2656 = VECTOR ( 'NONE', #7004, 1000.000000000000000 ) ;
#2657 = VERTEX_POINT ( 'NONE', #4542 ) ;
#2658 = EDGE_LOOP ( 'NONE', ( #13924, #14242 ) ) ;
#2659 = CARTESIAN_POINT ( 'NONE',  ( 4.078421086530217288, -3.990950201428958621, -1.000000000000000000 ) ) ;
#2660 = CIRCLE ( 'NONE', #16725, 1.000000000000002665 ) ;
#2661 = DIRECTION ( 'NONE',  ( -0.000000000000000000, -0.000000000000000000, 1.000000000000000000 ) ) ;
#2662 = DIRECTION ( 'NONE',  ( -0.03668796685672145313, 0.9993267699245927949, 2.695122805014889898E-17 ) ) ;
#2663 = EDGE_LOOP ( 'NONE', ( #1060, #3805, #8968, #3798, #151, #13906, #8954, #2568 ) ) ;
#2664 = FACE_OUTER_BOUND ( 'NONE', #10436, .T. ) ;
#2665 = VERTEX_POINT ( 'NONE', #1404 ) ;
#2666 = ORIENTED_EDGE ( 'NONE', *, *, #9256, .F. ) ;
#2667 = DIRECTION ( 'NONE',  ( 1.000000000000000000, 0.000000000000000000, 0.000000000000000000 ) ) ;
#2668 = DIRECTION ( 'NONE',  ( 0.000000000000000000, 0.000000000000000000, 1.000000000000000000 ) ) ;
#2669 = VECTOR ( 'NONE', #9989, 1000.000000000000000 ) ;
#2670 = CARTESIAN_POINT ( 'NONE',  ( 53.54508667620424234, 46.70051614449766220, -4.840751629271188961 ) ) ;
#2671 = DIRECTION ( 'NONE',  ( -1.000000000000000000, 0.000000000000000000, 0.000000000000000000 ) ) ;
#2672 = CARTESIAN_POINT ( 'NONE',  ( 4.175813232069147674, 2.061359961916367833, 3.570380186727398097 ) ) ;
#2673 = CARTESIAN_POINT ( 'NONE',  ( 55.11794222512601493, 54.19948385550241454, 3.688883143319541702 ) ) ;
#2674 = DIRECTION ( 'NONE',  ( 0.000000000000000000, -0.000000000000000000, 1.000000000000000000 ) ) ;
#2675 = CARTESIAN_POINT ( 'NONE',  ( 44.05948171654949874, 48.79948385550238754, 4.345558710429105354 ) ) ;
#2676 = CARTESIAN_POINT ( 'NONE',  ( 45.31609314410960820, 46.30051614449766362, -6.485486291978072693 ) ) ;
#2677 = CARTESIAN_POINT ( 'NONE',  ( 0.4465819873851989974, -2.886751345948120218, 4.999999999999999112 ) ) ;
#2678 = ORIENTED_EDGE ( 'NONE', *, *, #16129, .F. ) ;
#2679 = DIRECTION ( 'NONE',  ( 1.000000000000000000, 0.000000000000000000, 0.000000000000000000 ) ) ;
#2680 = CIRCLE ( 'NONE', #13918, 2.396904916527699214 ) ;
#2681 =( BOUNDED_SURFACE ( )  B_SPLINE_SURFACE ( 3, 2, ( 
 ( #6327, #4572, #13950 ),
 ( #4768, #247, #6505 ),
 ( #7690, #12102, #12481 ),
 ( #9167, #15058, #3207 ),
 ( #13767, #7600, #4942 ),
 ( #3291, #4856, #15147 ) ),
 .UNSPECIFIED., .F., .F., .F. ) 
 B_SPLINE_SURFACE_WITH_KNOTS ( ( 4, 2, 4 ),
 ( 3, 3 ),
 ( 0.02368235114939812314, 0.02663560780161266378, 0.02958886445382720443 ),
 ( 0.000000000000000000, 1.000000000000000000 ),
 .UNSPECIFIED. ) 
 GEOMETRIC_REPRESENTATION_ITEM ( )  RATIONAL_B_SPLINE_SURFACE ( (
 ( 1.000000000000000000, 0.8047780980783513227, 1.000000000000000000),
 ( 1.000000000000000000, 0.8123789398383446381, 1.000000000000000000),
 ( 1.000000000000000000, 0.8190677725692530053, 1.000000000000000000),
 ( 1.000000000000000000, 0.8192346316605858547, 1.000000000000000000),
 ( 1.000000000000000000, 0.8126126875065289301, 1.000000000000000000),
 ( 1.000000000000000000, 0.8047712635281869531, 1.000000000000000000) ) ) 
 REPRESENTATION_ITEM ( '' )  SURFACE ( )  );
#2682 = VERTEX_POINT ( 'NONE', #10501 ) ;
#2683 = VECTOR ( 'NONE', #17447, 1000.000000000000000 ) ;
#2684 = CARTESIAN_POINT ( 'NONE',  ( -3.453038570459499024, -2.625189405340453419, -3.535263753545272891 ) ) ;
#2685 = DIRECTION ( 'NONE',  ( 1.000000000000000000, 0.000000000000000000, -0.000000000000000000 ) ) ;
#2686 = AXIS2_PLACEMENT_3D ( 'NONE', #18484, #5033, #3563 ) ;
#2687 = CARTESIAN_POINT ( 'NONE',  ( 20.00000000000000000, -20.00000000000000000, -23.00000000000000000 ) ) ;
#2688 = CARTESIAN_POINT ( 'NONE',  ( 4.197393957002303999, 7.772902908466098641E-14, -3.503767560748929810 ) ) ;
#2689 = VERTEX_POINT ( 'NONE', #13645 ) ;
#2690 = CYLINDRICAL_SURFACE ( 'NONE', #5451, 0.7500000000000000000 ) ;
#2691 = CARTESIAN_POINT ( 'NONE',  ( 2.756197834950227410, 3.027510591568626896, -3.223146290109805356 ) ) ;
#2692 = CARTESIAN_POINT ( 'NONE',  ( 56.65037692655918988, 49.89948385550240317, -2.184720259617163762 ) ) ;
#2693 = PLANE ( 'NONE',  #16419 ) ;
#2694 = CARTESIAN_POINT ( 'NONE',  ( 42.39856655714564226, 64.10051614449766078, -2.493737253992044156 ) ) ;
#2695 = FACE_OUTER_BOUND ( 'NONE', #8011, .T. ) ;
#2696 = EDGE_CURVE ( 'NONE', #7605, #9351, #4641, .T. ) ;
#2697 = CARTESIAN_POINT ( 'NONE',  ( 49.97728705011495265, 49.50051614449765935, 7.000000000000000888 ) ) ;
#2698 = DIRECTION ( 'NONE',  ( -0.000000000000000000, -0.000000000000000000, -1.000000000000000000 ) ) ;
#2699 = AXIS2_PLACEMENT_3D ( 'NONE', #6753, #12737, #17071 ) ;
#2700 = VERTEX_POINT ( 'NONE', #6200 ) ;
#2701 = ADVANCED_FACE ( 'NONE', ( #16409 ), #3927, .F. ) ;
#2702 = ORIENTED_EDGE ( 'NONE', *, *, #5792, .T. ) ;
#2703 = DIRECTION ( 'NONE',  ( -0.000000000000000000, -0.000000000000000000, -1.000000000000000000 ) ) ;
#2704 = ORIENTED_EDGE ( 'NONE', *, *, #2799, .F. ) ;
#2705 = ADVANCED_FACE ( 'NONE', ( #1602, #10601 ), #7571, .F. ) ;
#2706 = ADVANCED_FACE ( 'NONE', ( #18078, #9137 ), #4740, .T. ) ;
#2707 = DIRECTION ( 'NONE',  ( 0.000000000000000000, 0.000000000000000000, -1.000000000000000000 ) ) ;
#2708 = ORIENTED_EDGE ( 'NONE', *, *, #15391, .T. ) ;
#2709 = CARTESIAN_POINT ( 'NONE',  ( 0.000000000000000000, 0.000000000000000000, -4.974599999999998801 ) ) ;
#2710 = EDGE_CURVE ( 'NONE', #442, #5017, #9444, .T. ) ;
#2711 = ORIENTED_EDGE ( 'NONE', *, *, #16035, .F. ) ;
#2712 = CARTESIAN_POINT ( 'NONE',  ( -4.688877333428353111, -21.02685410450703074, 9.999999999999998224 ) ) ;
#2713 = VERTEX_POINT ( 'NONE', #19373 ) ;
#2714 = CARTESIAN_POINT ( 'NONE',  ( 56.81924384183011512, 60.19948385550240744, 4.924951120819313743 ) ) ;
#2715 = FACE_OUTER_BOUND ( 'NONE', #15236, .T. ) ;
#2716 = CARTESIAN_POINT ( 'NONE',  ( 55.08986747509847248, 53.79948385550241596, -3.727524721679197572 ) ) ;
#2717 = DIRECTION ( 'NONE',  ( 1.000000000000000000, 0.000000000000000000, 0.000000000000000000 ) ) ;
#2718 = CARTESIAN_POINT ( 'NONE',  ( 50.00000000000000000, 15.00000000000000000, 0.000000000000000000 ) ) ;
#2719 = CARTESIAN_POINT ( 'NONE',  ( 52.62207051974829852, 46.60051614449764656, -7.992620115222797139 ) ) ;
#2720 = ADVANCED_FACE ( 'NONE', ( #18181 ), #8520, .T. ) ;
#2721 = CARTESIAN_POINT ( 'NONE',  ( 49.97728705011494554, 49.50051614449766646, 6.000000000000000888 ) ) ;
#2722 = AXIS2_PLACEMENT_3D ( 'NONE', #2861, #11750, #13233 ) ;
#2723 = EDGE_CURVE ( 'NONE', #1247, #2192, #18742, .T. ) ;
#2724 = CARTESIAN_POINT ( 'NONE',  ( -12.54977455159113475, -35.57251292194792569, 9.000000000000000000 ) ) ;
#2725 = DIRECTION ( 'NONE',  ( -1.000000000000000000, 0.000000000000000000, 1.224646799147353207E-16 ) ) ;
#2726 = ORIENTED_EDGE ( 'NONE', *, *, #5478, .F. ) ;
#2727 = ORIENTED_EDGE ( 'NONE', *, *, #6989, .T. ) ;
#2728 = LINE ( 'NONE', #5842, #16587 ) ;
#2729 = ORIENTED_EDGE ( 'NONE', *, *, #9965, .T. ) ;
#2730 = CARTESIAN_POINT ( 'NONE',  ( 49.97728705011488159, 57.49948385550241170, -7.000000000000000888 ) ) ;
#2731 = LINE ( 'NONE', #2918, #7805 ) ;
#2732 = EDGE_LOOP ( 'NONE', ( #5047, #2637, #10170 ) ) ;
#2733 = ORIENTED_EDGE ( 'NONE', *, *, #13332, .F. ) ;
#2734 = DIRECTION ( 'NONE',  ( 0.000000000000000000, 0.000000000000000000, -1.000000000000000000 ) ) ;
#2735 = DIRECTION ( 'NONE',  ( 0.000000000000000000, 0.000000000000000000, -1.000000000000000000 ) ) ;
#2736 = ORIENTED_EDGE ( 'NONE', *, *, #4601, .T. ) ;
#2737 = LINE ( 'NONE', #5658, #15697 ) ;
#2738 = EDGE_LOOP ( 'NONE', ( #12306, #18684, #5042, #5138, #9261 ) ) ;
#2739 = CARTESIAN_POINT ( 'NONE',  ( -0.5469614295416921346, 4.303013824936271270, -3.535263753543735454 ) ) ;
#2740 = CARTESIAN_POINT ( 'NONE',  ( 45.90387839640214196, 50.69948385550240744, 5.676469297603166098 ) ) ;
#2741 = DIRECTION ( 'NONE',  ( 1.000000000000000000, 0.000000000000000000, 0.000000000000000000 ) ) ;
#2742 = VECTOR ( 'NONE', #12153, 1000.000000000000000 ) ;
#2743 = CARTESIAN_POINT ( 'NONE',  ( 44.05948171654945611, 48.20051614449764799, -4.345558710429044069 ) ) ;
#2744 = CARTESIAN_POINT ( 'NONE',  ( 4.071447262713888016, -2.020725942163694722, -3.499999999999999556 ) ) ;
#2745 = DIRECTION ( 'NONE',  ( -4.082155997157844188E-16, 1.000000000000000000, 0.000000000000000000 ) ) ;
#2746 = DIRECTION ( 'NONE',  ( 0.000000000000000000, 0.000000000000000000, -1.000000000000000000 ) ) ;
#2747 = AXIS2_PLACEMENT_3D ( 'NONE', #10199, #16201, #14918 ) ;
#2748 = PRODUCT_DEFINITION_SHAPE ( 'NONE', 'NONE',  #3281 ) ;
#2749 = ORIENTED_EDGE ( 'NONE', *, *, #16843, .F. ) ;
#2750 = EDGE_LOOP ( 'NONE', ( #14452, #279, #17212, #18930 ) ) ;
#2751 = FACE_BOUND ( 'NONE', #7624, .T. ) ;
#2752 =( NAMED_UNIT ( * ) SI_UNIT ( $, .STERADIAN. ) SOLID_ANGLE_UNIT ( ) );
#2753 = CARTESIAN_POINT ( 'NONE',  ( 1.149999999999998135, 0.000000000000000000, 0.000000000000000000 ) ) ;
#2754 = EDGE_LOOP ( 'NONE', ( #9771, #4011, #9063, #7040 ) ) ;
#2755 = VECTOR ( 'NONE', #6736, 1000.000000000000000 ) ;
#2756 = CARTESIAN_POINT ( 'NONE',  ( 6.357976367241986893, 5.421935536069748096, 0.8264656814052228073 ) ) ;
#2757 = ORIENTED_EDGE ( 'NONE', *, *, #14030, .T. ) ;
#2758 = ORIENTED_EDGE ( 'NONE', *, *, #1011, .F. ) ;
#2759 = ADVANCED_FACE ( 'NONE', ( #8600 ), #5931, .F. ) ;
#2760 = CARTESIAN_POINT ( 'NONE',  ( -154.8532481325730998, -18.99730707969839116, 15.79999999999999893 ) ) ;
#2761 = CARTESIAN_POINT ( 'NONE',  ( 51.92680522751238925, 47.40051614449765793, 6.007379884777208190 ) ) ;
#2762 = CARTESIAN_POINT ( 'NONE',  ( 0.05140428708382910328, -4.819072548984009607, -1.653121499799246719 ) ) ;
#2763 = EDGE_CURVE ( 'NONE', #12835, #6920, #3511, .T. ) ;
#2764 = AXIS2_PLACEMENT_3D ( 'NONE', #9423, #9512, #6382 ) ;
#2765 = CARTESIAN_POINT ( 'NONE',  ( 46.45491332379572924, 53.29948385550240886, -4.840751629271157874 ) ) ;
#2766 = CYLINDRICAL_SURFACE ( 'NONE', #8184, 1.000000000000000000 ) ;
#2767 = VECTOR ( 'NONE', #19296, 1000.000000000000000 ) ;
#2768 = CARTESIAN_POINT ( 'NONE',  ( 56.65037692655918988, 49.89948385550240317, -2.184720259617163762 ) ) ;
#2769 = CARTESIAN_POINT ( 'NONE',  ( 54.72065718078918906, 44.70051614449765509, -6.458785618021089192 ) ) ;
#2770 = CARTESIAN_POINT ( 'NONE',  ( 0.01055556052338869899, -4.084588180558399451, 2.925285743277528105 ) ) ;
#2771 = CARTESIAN_POINT ( 'NONE',  ( 2.449293598294706513E-15, -20.00000000000000000, -23.00000000000000000 ) ) ;
#2772 = DIRECTION ( 'NONE',  ( 0.000000000000000000, 0.000000000000000000, 1.000000000000000000 ) ) ;
#2773 = VECTOR ( 'NONE', #14133, 1000.000000000000000 ) ;
#2774 = EDGE_LOOP ( 'NONE', ( #1993, #2634, #2415, #14369 ) ) ;
#2775 = LINE ( 'NONE', #17768, #7973 ) ;
#2776 = AXIS2_PLACEMENT_3D ( 'NONE', #14016, #5202, #15600 ) ;
#2777 = CYLINDRICAL_SURFACE ( 'NONE', #1885, 4.800000000000000711 ) ;
#2778 = CARTESIAN_POINT ( 'NONE',  ( 0.000000000000000000, 0.000000000000000000, 0.000000000000000000 ) ) ;
#2779 = DIRECTION ( 'NONE',  ( -0.000000000000000000, -0.000000000000000000, 1.000000000000000000 ) ) ;
#2780 = STYLED_ITEM ( 'NONE', ( #19131 ), #15256 ) ;
#2781 = CARTESIAN_POINT ( 'NONE',  ( -154.9999999999999716, -14.99999999999999645, -15.79999999999999538 ) ) ;
#2782 = LINE ( 'NONE', #18772, #6479 ) ;
#2783 = CARTESIAN_POINT ( 'NONE',  ( 52.29715082351547295, 54.39948385550239607, 6.992620115222774047 ) ) ;
#2784 = DIRECTION ( 'NONE',  ( 1.000000000000000000, 0.000000000000000000, 0.000000000000000000 ) ) ;
#2785 = CARTESIAN_POINT ( 'NONE',  ( 56.81924384183011512, 52.19948385550240744, 4.924951120819313743 ) ) ;
#2786 = CARTESIAN_POINT ( 'NONE',  ( -4.000000000000004441, 2.309401076758496263, -3.504269196027523847 ) ) ;
#2787 = CIRCLE ( 'NONE', #9951, 20.00000000000000000 ) ;
#2788 = CARTESIAN_POINT ( 'NONE',  ( 47.74827507625469281, 50.40051614449764372, -7.007379884777203749 ) ) ;
#2789 = VECTOR ( 'NONE', #15781, 1000.000000000000000 ) ;
#2790 = CARTESIAN_POINT ( 'NONE',  ( 20.00000000000000000, -20.00000000000000000, -20.00000000000000000 ) ) ;
#2791 = VERTEX_POINT ( 'NONE', #2170 ) ;
#2792 = VERTEX_POINT ( 'NONE', #11826 ) ;
#2793 = CYLINDRICAL_SURFACE ( 'NONE', #8418, 20.00000000000000000 ) ;
#2794 = VERTEX_POINT ( 'NONE', #4100 ) ;
#2795 = LINE ( 'NONE', #7482, #12483 ) ;
#2796 = ORIENTED_EDGE ( 'NONE', *, *, #6179, .F. ) ;
#2797 = FACE_OUTER_BOUND ( 'NONE', #5969, .T. ) ;
#2798 = AXIS2_PLACEMENT_3D ( 'NONE', #1754, #5071, #277 ) ;
#2799 = EDGE_CURVE ( 'NONE', #3316, #16533, #1007, .T. ) ;
#2800 = ORIENTED_EDGE ( 'NONE', *, *, #18948, .F. ) ;
#2801 = DIRECTION ( 'NONE',  ( -4.082155997157844188E-16, 1.000000000000000000, 0.000000000000000000 ) ) ;
#2802 = VERTEX_POINT ( 'NONE', #12743 ) ;
#2803 = CARTESIAN_POINT ( 'NONE',  ( 52.62207051974839089, 58.39948385550241028, 7.992620115222770494 ) ) ;
#2804 = FACE_OUTER_BOUND ( 'NONE', #13318, .T. ) ;
#2805 = CARTESIAN_POINT ( 'NONE',  ( 51.92680522751233951, 55.59948385550240602, -6.007379884777223289 ) ) ;
#2806 = PLANE ( 'NONE',  #12919 ) ;
#2807 = DIRECTION ( 'NONE',  ( -0.000000000000000000, 1.000000000000000000, -0.000000000000000000 ) ) ;
#2808 = PRESENTATION_LAYER_ASSIGNMENT (  '', '', ( #15318 ) ) ;
#2809 = CARTESIAN_POINT ( 'NONE',  ( 56.79116909180259398, 49.20051614449766220, 4.963592699178938972 ) ) ;
#2810 = CARTESIAN_POINT ( 'NONE',  ( 44.28664221472221385, 51.90051614449765793, 1.832500667257213722 ) ) ;
#2811 = FACE_OUTER_BOUND ( 'NONE', #15172, .T. ) ;
#2812 = CIRCLE ( 'NONE', #13129, 12.49999999999999645 ) ;
#2813 = ORIENTED_EDGE ( 'NONE', *, *, #14960, .F. ) ;
#2814 = AXIS2_PLACEMENT_3D ( 'NONE', #12299, #355, #16535 ) ;
#2815 = EDGE_CURVE ( 'NONE', #4950, #11986, #12899, .T. ) ;
#2816 = EDGE_CURVE ( 'NONE', #19190, #17340, #74, .T. ) ;
#2817 = ORIENTED_EDGE ( 'NONE', *, *, #176, .F. ) ;
#2818 = PLANE ( 'NONE',  #9336 ) ;
#2819 = VERTEX_POINT ( 'NONE', #14109 ) ;
#2820 = DIRECTION ( 'NONE',  ( 0.000000000000000000, 1.000000000000000000, 0.000000000000000000 ) ) ;
#2821 = CARTESIAN_POINT ( 'NONE',  ( 73.00000000000002842, -3.000000000000000000, 6.000000000000001776 ) ) ;
#2822 = AXIS2_PLACEMENT_3D ( 'NONE', #2535, #7015, #16146 ) ;
#2823 = ORIENTED_EDGE ( 'NONE', *, *, #17798, .F. ) ;
#2824 = CYLINDRICAL_SURFACE ( 'NONE', #11268, 20.00000000000000000 ) ;
#2825 = EDGE_CURVE ( 'NONE', #8729, #6112, #16066, .T. ) ;
#2826 = CARTESIAN_POINT ( 'NONE',  ( 55.96859303347805081, 46.19948385550240033, 4.306917132069425058 ) ) ;
#2827 = ADVANCED_FACE ( 'NONE', ( #2648 ), #1255, .F. ) ;
#2828 = VERTEX_POINT ( 'NONE', #3729 ) ;
#2829 = DIRECTION ( 'NONE',  ( 0.000000000000000000, 8.673617379884036458E-16, 1.000000000000000000 ) ) ;
#2830 = ORIENTED_EDGE ( 'NONE', *, *, #4507, .T. ) ;
#2831 = VECTOR ( 'NONE', #18960, 1000.000000000000000 ) ;
#2832 = DIRECTION ( 'NONE',  ( 0.000000000000000000, 0.000000000000000000, -1.000000000000000000 ) ) ;
#2833 = CARTESIAN_POINT ( 'NONE',  ( 43.34962307344081012, 48.89948385550240317, 2.184720259617164650 ) ) ;
#2834 = FACE_OUTER_BOUND ( 'NONE', #7295, .T. ) ;
#2835 = CARTESIAN_POINT ( 'NONE',  ( 47.70284917648459100, 49.60051614449763946, 6.992620115222796251 ) ) ;
#2836 = CARTESIAN_POINT ( 'NONE',  ( -19.89043790736545603, -22.09056926535314602, -9.000000000000000000 ) ) ;
#2837 = ADVANCED_FACE ( 'NONE', ( #13207 ), #6022, .T. ) ;
#2838 = CIRCLE ( 'NONE', #13770, 2.649999999999985700 ) ;
#2839 = EDGE_CURVE ( 'NONE', #4192, #18235, #11010, .T. ) ;
#2840 = CARTESIAN_POINT ( 'NONE',  ( 0.000000000000000000, 0.000000000000000000, 0.000000000000000000 ) ) ;
#2841 = EDGE_CURVE ( 'NONE', #7251, #10053, #7325, .T. ) ;
#2842 = VERTEX_POINT ( 'NONE', #4287 ) ;
#2843 = VERTEX_POINT ( 'NONE', #18653 ) ;
#2844 = CARTESIAN_POINT ( 'NONE',  ( -2.688821387764050996E-14, -4.618802153517012954, -0.4999999999999995559 ) ) ;
#2845 = AXIS2_PLACEMENT_3D ( 'NONE', #1881, #16783, #9309 ) ;
#2846 = CARTESIAN_POINT ( 'NONE',  ( 47.74827507625478518, 48.59948385550239180, 7.007379884777227730 ) ) ;
#2847 = DIRECTION ( 'NONE',  ( 1.000000000000000000, 0.000000000000000000, 0.000000000000000000 ) ) ;
#2848 = CIRCLE ( 'NONE', #9701, 20.00000000000000000 ) ;
#2849 = AXIS2_PLACEMENT_3D ( 'NONE', #7793, #16734, #10920 ) ;
#2850 = EDGE_LOOP ( 'NONE', ( #3388, #18980, #16443, #4274 ) ) ;
#2851 = FACE_OUTER_BOUND ( 'NONE', #1818, .T. ) ;
#2852 = CIRCLE ( 'NONE', #2236, 5.899999999999999467 ) ;
#2853 = ORIENTED_EDGE ( 'NONE', *, *, #5080, .T. ) ;
#2854 = VERTEX_POINT ( 'NONE', #14768 ) ;
#2855 = CARTESIAN_POINT ( 'NONE',  ( 2.449293598294706513E-15, -20.00000000000000000, 9.000000000000000000 ) ) ;
#2856 = UNCERTAINTY_MEASURE_WITH_UNIT (LENGTH_MEASURE( 1.000000000000000082E-05 ), #11966, 'distance_accuracy_value', 'NONE');
#2857 = CARTESIAN_POINT ( 'NONE',  ( 4.688877333453708829, -18.97314589549297281, 9.999999999999998224 ) ) ;
#2859 = AXIS2_PLACEMENT_3D ( 'NONE', #19237, #5483, #7155 ) ;
#2858 = CARTESIAN_POINT ( 'NONE',  ( 56.30877334542961421, 47.00051614449766646, 0.02388180880515774693 ) ) ;
#2860 = CYLINDRICAL_SURFACE ( 'NONE', #8608, 20.00000000000000000 ) ;
#2861 = CARTESIAN_POINT ( 'NONE',  ( -154.9999999999999716, -14.99999999999999645, 9.000000000000000000 ) ) ;
#2862 = CARTESIAN_POINT ( 'NONE',  ( 44.91013252490152752, 54.79948385550240175, 3.727524721679198461 ) ) ;
#2863 = VECTOR ( 'NONE', #9367, 1000.000000000000000 ) ;
#2864 = DIRECTION ( 'NONE',  ( -1.000000000000000000, -0.000000000000000000, -0.000000000000000000 ) ) ;
#2865 = CARTESIAN_POINT ( 'NONE',  ( 45.90387839640214196, 54.69948385550240744, 5.676469297603166098 ) ) ;
#2866 = CARTESIAN_POINT ( 'NONE',  ( 54.68390685589039890, 47.30051614449766362, 6.485486291978072693 ) ) ;
#2867 = CARTESIAN_POINT ( 'NONE',  ( 0.000000000000000000, -4.330127018922188320, 2.500000000000010214 ) ) ;
#2868 = CARTESIAN_POINT ( 'NONE',  ( -150.9999999999999432, -14.99999999999999645, 15.00000000000000000 ) ) ;
#2869 = EDGE_LOOP ( 'NONE', ( #12972, #17232, #17630, #3143 ) ) ;
#2870 = CARTESIAN_POINT ( 'NONE',  ( -151.2001253019789431, -14.96914097636792818, 15.00000000000000000 ) ) ;
#2871 = CARTESIAN_POINT ( 'NONE',  ( 0.000000000000000000, 0.000000000000000000, 0.000000000000000000 ) ) ;
#2872 = EDGE_CURVE ( 'NONE', #7670, #17070, #14138, .T. ) ;
#2873 = DIRECTION ( 'NONE',  ( -0.9931793912140981506, -0.1165962986873662205, 0.000000000000000000 ) ) ;
#2874 = VERTEX_POINT ( 'NONE', #6338 ) ;
#2875 = CARTESIAN_POINT ( 'NONE',  ( 2.449293598294706513E-15, -20.00000000000000000, 9.000000000000000000 ) ) ;
#2876 = EDGE_CURVE ( 'NONE', #162, #9683, #13779, .T. ) ;
#2877 = DIRECTION ( 'NONE',  ( 0.000000000000000000, 0.000000000000000000, 1.000000000000000000 ) ) ;
#2878 = AXIS2_PLACEMENT_3D ( 'NONE', #13205, #2829, #8398 ) ;
#2879 = CIRCLE ( 'NONE', #12555, 4.424999999999999822 ) ;
#2880 = DIRECTION ( 'NONE',  ( -0.000000000000000000, -0.000000000000000000, 1.000000000000000000 ) ) ;
#2881 = DIRECTION ( 'NONE',  ( -1.000000000000000000, 0.000000000000000000, 0.000000000000000000 ) ) ;
#2882 = CYLINDRICAL_SURFACE ( 'NONE', #11472, 12.49999999999999645 ) ;
#2883 = DIRECTION ( 'NONE',  ( 1.000000000000000000, 0.000000000000000000, 0.000000000000000000 ) ) ;
#2884 = CARTESIAN_POINT ( 'NONE',  ( 75.00000000000001421, -7.499999999999971578, -20.00000000000000000 ) ) ;
#2885 = CARTESIAN_POINT ( 'NONE',  ( 56.66441430157296821, 56.09948385550240602, 2.141517661632100111 ) ) ;
#2886 = FACE_OUTER_BOUND ( 'NONE', #3109, .T. ) ;
#2887 = CARTESIAN_POINT ( 'NONE',  ( 49.97728705011486738, 53.49948385550240459, -8.000000000000001776 ) ) ;
#2888 = APPLICATION_CONTEXT ( 'automotive_design' ) ;
#2889 = CARTESIAN_POINT ( 'NONE',  ( 4.086376042167608524, -4.082715877136868343, 0.07147133206917789805 ) ) ;
#2890 = CARTESIAN_POINT ( 'NONE',  ( 47.74827507625469281, 46.40051614449764372, -7.007379884777203749 ) ) ;
#2891 = DIRECTION ( 'NONE',  ( 1.000000000000000000, 0.000000000000000000, 0.000000000000000000 ) ) ;
#2892 = VERTEX_POINT ( 'NONE', #13592 ) ;
#2893 = EDGE_LOOP ( 'NONE', ( #14519, #1241, #8781, #541, #15083, #16639, #1361, #2418, #6160, #17930, #16178, #3967 ) ) ;
#2894 = CARTESIAN_POINT ( 'NONE',  ( 5.599999999999999645, -2.020725942163686284, 3.500000000000000444 ) ) ;
#2895 = EDGE_LOOP ( 'NONE', ( #13031, #2901 ) ) ;
#2896 = CARTESIAN_POINT ( 'NONE',  ( 0.000000000000000000, 0.8865213383406715941, 1.535499999999999199 ) ) ;
#2897 = VERTEX_POINT ( 'NONE', #260 ) ;
#2898 = DIRECTION ( 'NONE',  ( 0.000000000000000000, 0.000000000000000000, 1.000000000000000000 ) ) ;
#2899 = ORIENTED_EDGE ( 'NONE', *, *, #5076, .T. ) ;
#2900 = DIRECTION ( 'NONE',  ( -1.000000000000000000, 0.000000000000000000, 0.000000000000000000 ) ) ;
#2901 = ORIENTED_EDGE ( 'NONE', *, *, #17364, .F. ) ;
#2902 = DIRECTION ( 'NONE',  ( 0.000000000000000000, 1.000000000000000000, -1.345283343056720273E-15 ) ) ;
#2903 = CARTESIAN_POINT ( 'NONE',  ( -10.93224627749309796, -3.252283996668732691, 9.000000000000000000 ) ) ;
#2904 = PRODUCT_DEFINITION_SHAPE ( 'NONE', 'NONE',  #19428 ) ;
#2905 = CARTESIAN_POINT ( 'NONE',  ( 44.28664221472220675, 57.09948385550240602, -1.832500667257165317 ) ) ;
#2906 = CARTESIAN_POINT ( 'NONE',  ( 0.000000000000000000, -4.330127018922188320, 2.500000000000010214 ) ) ;
#2907 = DIRECTION ( 'NONE',  ( 1.000000000000000000, 0.000000000000000000, 0.000000000000000000 ) ) ;
#2908 = CARTESIAN_POINT ( 'NONE',  ( 54.68390685589039890, 51.30051614449765651, 6.485486291978072693 ) ) ;
#2909 = CARTESIAN_POINT ( 'NONE',  ( 55.11794222512599362, 48.80051614449767072, -3.688883143319583446 ) ) ;
#2910 = CARTESIAN_POINT ( 'NONE',  ( -154.9999999999999716, -14.99999999999999645, 15.79999999999999893 ) ) ;
#2911 = FACE_OUTER_BOUND ( 'NONE', #4695, .T. ) ;
#2912 = ORIENTED_EDGE ( 'NONE', *, *, #4144, .F. ) ;
#2913 = AXIS2_PLACEMENT_3D ( 'NONE', #17621, #11508, #17325 ) ;
#2914 = ORIENTED_EDGE ( 'NONE', *, *, #9264, .T. ) ;
#2915 = CARTESIAN_POINT ( 'NONE',  ( 0.000000000000000000, 0.000000000000000000, 0.000000000000000000 ) ) ;
#2916 = EDGE_LOOP ( 'NONE', ( #12928, #16925, #9402, #12399, #16147, #13199 ) ) ;
#2917 = PLANE ( 'NONE',  #18962 ) ;
#2918 = CARTESIAN_POINT ( 'NONE',  ( -154.8605857259444463, -18.79744172571344762, 15.00000000000000000 ) ) ;
#2919 = ORIENTED_EDGE ( 'NONE', *, *, #14071, .T. ) ;
#2920 = DIRECTION ( 'NONE',  ( -0.000000000000000000, -0.000000000000000000, -1.000000000000000000 ) ) ;
#2921 = DIRECTION ( 'NONE',  ( 0.000000000000000000, 1.000000000000000000, 0.000000000000000000 ) ) ;
#2922 = ORIENTED_EDGE ( 'NONE', *, *, #15885, .T. ) ;
#2923 = FACE_OUTER_BOUND ( 'NONE', #2750, .T. ) ;
#2924 = ORIENTED_EDGE ( 'NONE', *, *, #15484, .T. ) ;
#2925 = CARTESIAN_POINT ( 'NONE',  ( 51.51576781266200555, 45.00000000000000711, -6.337576802645323859 ) ) ;
#2926 = CARTESIAN_POINT ( 'NONE',  ( 42.63976443033212860, 58.99948385550239038, 0.02388180880522514787 ) ) ;
#2927 = CARTESIAN_POINT ( 'NONE',  ( 0.000000000000000000, 0.000000000000000000, 0.000000000000000000 ) ) ;
#2928 = EDGE_CURVE ( 'NONE', #16215, #2657, #1646, .T. ) ;
#2929 = CARTESIAN_POINT ( 'NONE',  ( 54.13287192849671214, 52.70051614449766220, -5.649768623646139964 ) ) ;
#2930 = LINE ( 'NONE', #13404, #14835 ) ;
#2931 =( NAMED_UNIT ( * ) PLANE_ANGLE_UNIT ( ) SI_UNIT ( $, .RADIAN. ) );
#2932 = CARTESIAN_POINT ( 'NONE',  ( 75.00000000000000000, 32.50000000000001421, -15.00000000000000000 ) ) ;
#2933 = ORIENTED_EDGE ( 'NONE', *, *, #11365, .F. ) ;
#2934 = ADVANCED_FACE ( 'NONE', ( #1545 ), #3305, .T. ) ;
#2935 = ORIENTED_EDGE ( 'NONE', *, *, #2601, .T. ) ;
#2936 = ORIENTED_EDGE ( 'NONE', *, *, #6489, .T. ) ;
#2937 = CARTESIAN_POINT ( 'NONE',  ( 62.49999999999998579, 45.00000000000001421, 9.999999999999998224 ) ) ;
#2938 = EDGE_CURVE ( 'NONE', #13867, #585, #1651, .T. ) ;
#2939 = CARTESIAN_POINT ( 'NONE',  ( 47.37792948025162332, 63.39948385550238896, -7.992620115222770494 ) ) ;
#2940 = VERTEX_POINT ( 'NONE', #7703 ) ;
#2941 = DIRECTION ( 'NONE',  ( -0.000000000000000000, -0.000000000000000000, -1.000000000000000000 ) ) ;
#2942 = EDGE_CURVE ( 'NONE', #17307, #18471, #10397, .T. ) ;
#2943 = EDGE_CURVE ( 'NONE', #7410, #9683, #9451, .T. ) ;
#2944 = EDGE_LOOP ( 'NONE', ( #268, #2702, #9574, #11135, #8690 ) ) ;
#2945 = CARTESIAN_POINT ( 'NONE',  ( 43.33558569842706021, 57.90051614449766504, 2.141517661632167169 ) ) ;
#2946 = VERTEX_POINT ( 'NONE', #16451 ) ;
#2947 = DIRECTION ( 'NONE',  ( 0.000000000000000000, 0.000000000000000000, 1.000000000000000000 ) ) ;
#2948 = CYLINDRICAL_SURFACE ( 'NONE', #12723, 0.7500000000000000000 ) ;
#2949 = CARTESIAN_POINT ( 'NONE',  ( 55.71335778527780036, 46.90051614449766504, -1.832500667257213056 ) ) ;
#2950 = CARTESIAN_POINT ( 'NONE',  ( 5.599999999999999645, 2.020725942163686284, -3.499999999999999556 ) ) ;
#2951 = AXIS2_PLACEMENT_3D ( 'NONE', #4359, #12092, #19393 ) ;
#2952 = CARTESIAN_POINT ( 'NONE',  ( 0.000000000000000000, 0.4273491293402468805, 0.000000000000000000 ) ) ;
#2953 = CARTESIAN_POINT ( 'NONE',  ( 46.49166364869460466, 54.69948385550240033, 4.867452303228209765 ) ) ;
#2954 = PLANE ( 'NONE',  #12880 ) ;
#2955 = CARTESIAN_POINT ( 'NONE',  ( 47.74827507625478518, 54.59948385550239180, 7.007379884777227730 ) ) ;
#2956 = AXIS2_PLACEMENT_3D ( 'NONE', #173, #6148, #18677 ) ;
#2957 = EDGE_CURVE ( 'NONE', #2433, #6630, #8982, .T. ) ;
#2958 = CARTESIAN_POINT ( 'NONE',  ( 58.41169779390614281, 55.00051614449766646, 0.02388180880515032231 ) ) ;
#2959 = CARTESIAN_POINT ( 'NONE',  ( 4.158413352280807551, -2.044871626972826650, -3.541821552872960410 ) ) ;
#2960 = CARTESIAN_POINT ( 'NONE',  ( 3.950241966887845457, 3.393956070637746514, -1.121495646998088569 ) ) ;
#2961 = EDGE_CURVE ( 'NONE', #10552, #3811, #14966, .T. ) ;
#2962 = CARTESIAN_POINT ( 'NONE',  ( -74.99999999999997158, 2.999999999999999112, -20.00000000000000000 ) ) ;
#2963 = FILL_AREA_STYLE ('',( #16396 ) ) ;
#2964 = APPLICATION_PROTOCOL_DEFINITION ( 'draft international standard', 'automotive_design', 1998, #12402 ) ;
#2965 = ORIENTED_EDGE ( 'NONE', *, *, #10349, .F. ) ;
#2966 = FACE_OUTER_BOUND ( 'NONE', #12713, .T. ) ;
#2967 = VECTOR ( 'NONE', #17100, 1000.000000000000000 ) ;
#2968 = CARTESIAN_POINT ( 'NONE',  ( -0.1085714285714285687, -3.798448662927795372, -0.8000000000000000444 ) ) ;
#2969 = CARTESIAN_POINT ( 'NONE',  ( -1.393927851585477606, 4.043713361053528743, -3.526374918436835149 ) ) ;
#2970 = CARTESIAN_POINT ( 'NONE',  ( 6.481779955677433591, 2.910222513313285742, 5.040653254389411586 ) ) ;
#2971 = CARTESIAN_POINT ( 'NONE',  ( 20.00000000000000000, -20.00000000000000000, -12.00000000000000000 ) ) ;
#2972 = FACE_OUTER_BOUND ( 'NONE', #17073, .T. ) ;
#2973 = CARTESIAN_POINT ( 'NONE',  ( 45.90387839640214196, 60.69948385550240033, 5.676469297603166098 ) ) ;
#2974 = CYLINDRICAL_SURFACE ( 'NONE', #13266, 0.7500000000000000000 ) ;
#2975 = CARTESIAN_POINT ( 'NONE',  ( 42.39856655714566358, 52.89948385550241028, 2.493737253992119207 ) ) ;
#2976 = CARTESIAN_POINT ( 'NONE',  ( 3.948103430090710297, -3.379418997638724331, -1.146674596026246551 ) ) ;
#2977 = CARTESIAN_POINT ( 'NONE',  ( 44.03140696652198471, 57.80051614449766362, 4.306917132069485454 ) ) ;
#2978 = EDGE_CURVE ( 'NONE', #6396, #15249, #9141, .T. ) ;
#2979 = DIRECTION ( 'NONE',  ( -1.000000000000000000, 0.000000000000000000, 0.000000000000000000 ) ) ;
#2980 = CIRCLE ( 'NONE', #7969, 4.799999999999999822 ) ;
#2981 = ORIENTED_EDGE ( 'NONE', *, *, #7617, .T. ) ;
#2982 = ADVANCED_FACE ( 'NONE', ( #15072 ), #1739, .T. ) ;
#2983 = SURFACE_STYLE_USAGE ( .BOTH. , #10055 ) ;
#2984 = ORIENTED_EDGE ( 'NONE', *, *, #12318, .T. ) ;
#2985 = ORIENTED_EDGE ( 'NONE', *, *, #1313, .T. ) ;
#2986 = MECHANICAL_DESIGN_GEOMETRIC_PRESENTATION_REPRESENTATION (  '', ( #8613 ), #1740 ) ;
#2987 = CARTESIAN_POINT ( 'NONE',  ( 14.00000000000000000, 15.00000000000001776, 9.000000000000000000 ) ) ;
#2988 = ORIENTED_EDGE ( 'NONE', *, *, #6675, .F. ) ;
#2989 = CARTESIAN_POINT ( 'NONE',  ( -154.9999999999999716, -14.99999999999999645, -9.000000000000000000 ) ) ;
#2990 = EDGE_LOOP ( 'NONE', ( #14866, #3846 ) ) ;
#2991 = AXIS2_PLACEMENT_3D ( 'NONE', #18459, #213, #18562 ) ;
#2992 = DIRECTION ( 'NONE',  ( -4.082155997157844188E-16, 1.000000000000000000, 0.000000000000000000 ) ) ;
#2993 = VERTEX_POINT ( 'NONE', #6143 ) ;
#2994 = CARTESIAN_POINT ( 'NONE',  ( 2.000000000000008882, 3.464101615137749945, 0.000000000000000000 ) ) ;
#2995 = LINE ( 'NONE', #16522, #5436 ) ;
#2996 = EDGE_CURVE ( 'NONE', #8876, #2621, #15399, .T. ) ;
#2997 = CARTESIAN_POINT ( 'NONE',  ( 51.92680522751233951, 59.59948385550240602, -6.007379884777223289 ) ) ;
#2998 = DIRECTION ( 'NONE',  ( 1.000000000000000000, 0.000000000000000000, 0.000000000000000000 ) ) ;
#2999 = FILL_AREA_STYLE ('',( #16430 ) ) ;
#3000 = CARTESIAN_POINT ( 'NONE',  ( 47.37792948025170858, 53.60051614449765367, 7.992620115222797139 ) ) ;
#3001 = CIRCLE ( 'NONE', #4565, 0.9999999999999995559 ) ;
#3002 = ADVANCED_FACE ( 'NONE', ( #368 ), #4778, .F. ) ;
#3003 = CARTESIAN_POINT ( 'NONE',  ( 44.30067958973594955, 58.10051614449765367, -1.875703265242155693 ) ) ;
#3004 = CARTESIAN_POINT ( 'NONE',  ( -8.134732861515892921, -38.27090915285207018, 9.000000000000000000 ) ) ;
#3005 = CARTESIAN_POINT ( 'NONE',  ( 1.249999999999998002, 4.100000000000000533, 0.000000000000000000 ) ) ;
#3006 = ORIENTED_EDGE ( 'NONE', *, *, #10604, .F. ) ;
#3007 = ORIENTED_EDGE ( 'NONE', *, *, #4947, .F. ) ;
#3008 = LINE ( 'NONE', #17631, #16571 ) ;
#3009 = ORIENTED_EDGE ( 'NONE', *, *, #14539, .T. ) ;
#3010 = CARTESIAN_POINT ( 'NONE',  ( 45.90387839640214196, 62.69948385550240744, 5.676469297603166098 ) ) ;
#3011 = DIRECTION ( 'NONE',  ( 1.000000000000000000, 0.000000000000000000, 0.000000000000000000 ) ) ;
#3012 = ORIENTED_EDGE ( 'NONE', *, *, #6302, .F. ) ;
#3013 = CARTESIAN_POINT ( 'NONE',  ( 0.000000000000000000, 0.000000000000000000, 0.000000000000000000 ) ) ;
#3014 = CIRCLE ( 'NONE', #13941, 3.799999999999999378 ) ;
#3015 = CARTESIAN_POINT ( 'NONE',  ( 49.97728705011488159, 45.49948385550240459, -7.000000000000000888 ) ) ;
#3016 = ORIENTED_EDGE ( 'NONE', *, *, #6565, .F. ) ;
#3017 = DIRECTION ( 'NONE',  ( -0.000000000000000000, -0.000000000000000000, -1.000000000000000000 ) ) ;
#3018 = EDGE_LOOP ( 'NONE', ( #15293, #8632, #3138, #6074 ) ) ;
#3019 = CARTESIAN_POINT ( 'NONE',  ( 49.97728705011495265, 63.50051614449765935, 8.000000000000001776 ) ) ;
#3020 = CARTESIAN_POINT ( 'NONE',  ( 53.61415392313774220, 44.99999999999997868, -5.449226822604907206 ) ) ;
#3021 = CARTESIAN_POINT ( 'NONE',  ( 43.34962307344081012, 54.89948385550240317, 2.184720259617164650 ) ) ;
#3022 = CARTESIAN_POINT ( 'NONE',  ( -1.249999999999997780, 0.000000000000000000, -4.100000000000000533 ) ) ;
#3023 =( GEOMETRIC_REPRESENTATION_CONTEXT ( 3 ) GLOBAL_UNCERTAINTY_ASSIGNED_CONTEXT ( ( #12448 ) ) GLOBAL_UNIT_ASSIGNED_CONTEXT ( ( #5376, #17448, #3912 ) ) REPRESENTATION_CONTEXT ( 'NONE', 'WORKASPACE' ) );
#3024 = SURFACE_STYLE_FILL_AREA ( #18318 ) ;
#3025 = CARTESIAN_POINT ( 'NONE',  ( 55.96859303347802239, 56.80051614449764230, -4.306917132069484566 ) ) ;
#3026 = DIRECTION ( 'NONE',  ( -1.000000000000000000, 0.000000000000000000, 0.000000000000000000 ) ) ;
#3027 = FACE_OUTER_BOUND ( 'NONE', #15849, .T. ) ;
#3028 = CARTESIAN_POINT ( 'NONE',  ( 0.9996874511566293808, -39.97499999999999432, -9.000000000000000000 ) ) ;
#3029 = ORIENTED_EDGE ( 'NONE', *, *, #7729, .T. ) ;
#3030 = VERTEX_POINT ( 'NONE', #7423 ) ;
#3031 =( REPRESENTATION_RELATIONSHIP ('NONE','NONE', #16703, #17450 ) REPRESENTATION_RELATIONSHIP_WITH_TRANSFORMATION ( #6660 )SHAPE_REPRESENTATION_RELATIONSHIP( ) );
#3032 = VERTEX_POINT ( 'NONE', #13400 ) ;
#3033 = CARTESIAN_POINT ( 'NONE',  ( -6.315157543962389260E-16, -3.838309248099061044, -3.351853367130940065 ) ) ;
#3034 = CARTESIAN_POINT ( 'NONE',  ( 52.25172492374522903, 47.59948385550239891, -7.007379884777225953 ) ) ;
#3035 =( LENGTH_UNIT ( ) NAMED_UNIT ( * ) SI_UNIT ( .MILLI., .METRE. ) );
#3036 = ORIENTED_EDGE ( 'NONE', *, *, #16349, .F. ) ;
#3037 = DIRECTION ( 'NONE',  ( 0.000000000000000000, 1.224646799147353207E-16, 1.000000000000000000 ) ) ;
#3038 = ORIENTED_EDGE ( 'NONE', *, *, #11713, .F. ) ;
#3039 = CARTESIAN_POINT ( 'NONE',  ( 45.86712807150329496, 57.70051614449765509, 5.649768623646139964 ) ) ;
#3040 = ORIENTED_EDGE ( 'NONE', *, *, #17118, .T. ) ;
#3041 = CIRCLE ( 'NONE', #18383, 5.000000000000000888 ) ;
#3042 = EDGE_CURVE ( 'NONE', #8991, #13296, #3589, .T. ) ;
#3043 = CARTESIAN_POINT ( 'NONE',  ( -74.99999999999997158, -1.000000000000000000, -5.999999999999998224 ) ) ;
#3044 = PRODUCT_DEFINITION_CONTEXT ( 'detailed design', #11656, 'design' ) ;
#3045 = CARTESIAN_POINT ( 'NONE',  ( 4.030867648406620596, -2.329326259789657350, 2.965488570640411492 ) ) ;
#3046 = PRODUCT_DEFINITION ( 'UNKNOWN', '', #1988, #8910 ) ;
#3047 = CARTESIAN_POINT ( 'NONE',  ( 49.97728705011494554, 53.50051614449767357, 6.000000000000000888 ) ) ;
#3048 = DIRECTION ( 'NONE',  ( 0.03086419753086420623, 0.9995235871707959241, 0.000000000000000000 ) ) ;
#3049 = ADVANCED_FACE ( 'NONE', ( #15446 ), #8029, .F. ) ;
#3050 = CLOSED_SHELL ( 'NONE', ( #11551, #12818, #12677, #16496, #16720, #7692, #5212, #9043, #16819, #4658, #7547, #13586, #5565, #10107, #11468, #16105, #7593, #15278, #14470, #2131, #1006, #14914, #5238, #17940, #13003, #905, #6926, #658, #10337, #18770, #8668, #8209, #4637, #10878, #8572, #15621, #16901, #15242, #8795, #15598 ) ) ;
#3051 = CARTESIAN_POINT ( 'NONE',  ( -154.9999999999999716, -14.99999999999999645, -15.00000000000000000 ) ) ;
#3052 = CARTESIAN_POINT ( 'NONE',  ( 44.28664221472220675, 57.09948385550240602, -1.832500667257165317 ) ) ;
#3053 = CARTESIAN_POINT ( 'NONE',  ( 45.60000000000000142, 0.000000000000000000, 0.000000000000000000 ) ) ;
#3054 = CARTESIAN_POINT ( 'NONE',  ( 43.18075615816994173, 55.80051614449766362, 4.924951120819380357 ) ) ;
#3055 = EDGE_CURVE ( 'NONE', #19088, #6925, #8275, .T. ) ;
#3056 = CARTESIAN_POINT ( 'NONE',  ( 1.925929944387235853E-31, 15.00000000000001599, -9.000000000000001776 ) ) ;
#3057 = EDGE_CURVE ( 'NONE', #9040, #13819, #753, .T. ) ;
#3058 = VECTOR ( 'NONE', #18196, 1000.000000000000000 ) ;
#3059 = CARTESIAN_POINT ( 'NONE',  ( 4.180231891692620216, 4.134807952925572572, 0.02076457676760539231 ) ) ;
#3060 = DIRECTION ( 'NONE',  ( -1.000000000000000000, -0.000000000000000000, 0.000000000000000000 ) ) ;
#3061 = VECTOR ( 'NONE', #15468, 1000.000000000000000 ) ;
#3062 = EDGE_CURVE ( 'NONE', #10814, #11786, #3397, .T. ) ;
#3063 = CARTESIAN_POINT ( 'NONE',  ( -54.99999999999995737, -14.99999999999998579, -20.00000000000000000 ) ) ;
#3064 = VERTEX_POINT ( 'NONE', #18508 ) ;
#3065 = CARTESIAN_POINT ( 'NONE',  ( 0.3126073911695746443, -2.020725942163797750, -3.499999999999999556 ) ) ;
#3066 = DIRECTION ( 'NONE',  ( 1.000000000000000000, -0.000000000000000000, 0.000000000000000000 ) ) ;
#3067 = AXIS2_PLACEMENT_3D ( 'NONE', #14328, #11584, #15815 ) ;
#3068 = ADVANCED_FACE ( 'NONE', ( #10831 ), #18798, .F. ) ;
#3069 = AXIS2_PLACEMENT_3D ( 'NONE', #10990, #3551, #16996 ) ;
#3070 = CARTESIAN_POINT ( 'NONE',  ( 50.02271294988512551, 64.49948385550240459, 7.000000000000000888 ) ) ;
#3071 = EDGE_CURVE ( 'NONE', #16560, #9875, #17124, .T. ) ;
#3072 = CARTESIAN_POINT ( 'NONE',  ( 6.420058897733091463, 2.891482565094592339, 5.008194711943422028 ) ) ;
#3073=STYLED_ITEM('',(#19461),#8428);
#3074 = CARTESIAN_POINT ( 'NONE',  ( -6.473970235329672780E-16, -4.862606272033106691, -3.745885042887442395 ) ) ;
#3075 = DIRECTION ( 'NONE',  ( 0.000000000000000000, 0.000000000000000000, -1.000000000000000000 ) ) ;
#3076 = CARTESIAN_POINT ( 'NONE',  ( 52.25172492374522903, 59.59948385550240602, -7.007379884777225953 ) ) ;
#3077 = CARTESIAN_POINT ( 'NONE',  ( -62.49999999999997158, 32.50000000000001421, -15.00000000000000000 ) ) ;
#3078 = CARTESIAN_POINT ( 'NONE',  ( 58.41169779390614281, 51.99948385550239749, -0.02388180880523160798 ) ) ;
#3079 = CARTESIAN_POINT ( 'NONE',  ( 4.033901012035484790, -2.321269032827465661, -2.979444097106959788 ) ) ;
#3080 = CARTESIAN_POINT ( 'NONE',  ( 49.97728705011495265, 53.50051614449765935, 7.000000000000000888 ) ) ;
#3081 = EDGE_CURVE ( 'NONE', #3823, #4857, #6620, .T. ) ;
#3082 = AXIS2_PLACEMENT_3D ( 'NONE', #2397, #8350, #14521 ) ;
#3083 = DIRECTION ( 'NONE',  ( 0.000000000000000000, 0.000000000000000000, 1.000000000000000000 ) ) ;
#3084 = ORIENTED_EDGE ( 'NONE', *, *, #19242, .T. ) ;
#3085 = VECTOR ( 'NONE', #17867, 1000.000000000000000 ) ;
#3086 = FILL_AREA_STYLE ('',( #1506 ) ) ;
#3087 = VERTEX_POINT ( 'NONE', #15643 ) ;
#3088 = CARTESIAN_POINT ( 'NONE',  ( 6.385552186430389021, 2.886751345948122438, -5.000000000000001776 ) ) ;
#3089 = ORIENTED_EDGE ( 'NONE', *, *, #18187, .T. ) ;
#3090 = DIRECTION ( 'NONE',  ( 1.000000000000000000, 0.000000000000000000, 0.000000000000000000 ) ) ;
#3091 = CARTESIAN_POINT ( 'NONE',  ( 55.94051828345050836, 63.79948385550240886, -4.345558710429104465 ) ) ;
#3092 = CARTESIAN_POINT ( 'NONE',  ( 50.02271294988505446, 44.50051614449765935, -7.000000000000000888 ) ) ;
#3093 = ORIENTED_EDGE ( 'NONE', *, *, #12040, .T. ) ;
#3094 = DIRECTION ( 'NONE',  ( -0.000000000000000000, -0.000000000000000000, 1.000000000000000000 ) ) ;
#3095 = AXIS2_PLACEMENT_3D ( 'NONE', #17267, #15977, #11647 ) ;
#3096 = DIRECTION ( 'NONE',  ( 1.000000000000000000, 0.000000000000000000, 0.000000000000000000 ) ) ;
#3097 = AXIS2_PLACEMENT_3D ( 'NONE', #13122, #9094, #19329 ) ;
#3098 = CARTESIAN_POINT ( 'NONE',  ( 44.88205777487398507, 55.19948385550240744, -3.688883143319540814 ) ) ;
#3099 = LINE ( 'NONE', #1426, #19207 ) ;
#3100 = CARTESIAN_POINT ( 'NONE',  ( 0.04320752586819883584, 0.9836842030436125928, -5.000000000000000000 ) ) ;
#3101 = CARTESIAN_POINT ( 'NONE',  ( 52.57664461997821093, 55.40051614449767214, 8.007379884777206414 ) ) ;
#3102 = CARTESIAN_POINT ( 'NONE',  ( 44.30067958973594955, 54.10051614449766078, -1.875703265242155693 ) ) ;
#3103 = STYLED_ITEM ( 'NONE', ( #6949 ), #11988 ) ;
#3104 = CARTESIAN_POINT ( 'NONE',  ( 3.973110223767137850, -2.261493176400255405E-11, -3.565797985667433334 ) ) ;
#3105 = CARTESIAN_POINT ( 'NONE',  ( -3.333333333333335258, 2.694301256218251783, -3.300726591567079815 ) ) ;
#3106 = ORIENTED_EDGE ( 'NONE', *, *, #15806, .T. ) ;
#3107 = ORIENTED_EDGE ( 'NONE', *, *, #2341, .F. ) ;
#3108 = DIRECTION ( 'NONE',  ( -0.000000000000000000, -0.000000000000000000, -1.000000000000000000 ) ) ;
#3109 = EDGE_LOOP ( 'NONE', ( #11397, #15758, #16976, #14277 ) ) ;
#3110 = EDGE_CURVE ( 'NONE', #12100, #928, #7987, .T. ) ;
#3111 = CIRCLE ( 'NONE', #18453, 1.535500000000000087 ) ;
#3112 = CARTESIAN_POINT ( 'NONE',  ( 55.94051828345050836, 61.79948385550239465, -4.345558710429104465 ) ) ;
#3113 =( NAMED_UNIT ( * ) PLANE_ANGLE_UNIT ( ) SI_UNIT ( $, .RADIAN. ) );
#3114 = ORIENTED_EDGE ( 'NONE', *, *, #1758, .F. ) ;
#3115 = FACE_OUTER_BOUND ( 'NONE', #4698, .T. ) ;
#3116 = ADVANCED_FACE ( 'NONE', ( #643 ), #18619, .T. ) ;
#3117 = DIRECTION ( 'NONE',  ( 0.000000000000000000, 0.000000000000000000, 1.000000000000000000 ) ) ;
#3118 = ORIENTED_EDGE ( 'NONE', *, *, #5317, .F. ) ;
#3119 = CARTESIAN_POINT ( 'NONE',  ( -160.9999999999999432, -14.99999999999999645, -6.499999999999999112 ) ) ;
#3120 = ORIENTED_EDGE ( 'NONE', *, *, #3205, .F. ) ;
#3121 = CARTESIAN_POINT ( 'NONE',  ( 50.02271294988505446, 64.50051614449766646, -8.000000000000001776 ) ) ;
#3122 = CARTESIAN_POINT ( 'NONE',  ( -20.63749999999999574, 0.000000000000000000, 0.000000000000000000 ) ) ;
#3123 = CARTESIAN_POINT ( 'NONE',  ( 56.65037692655918988, 59.89948385550241028, -2.184720259617163762 ) ) ;
#3124 = DIRECTION ( 'NONE',  ( 1.000000000000000000, 0.000000000000000000, 0.000000000000000000 ) ) ;
#3125 = LINE ( 'NONE', #15355, #8048 ) ;
#3126 = CARTESIAN_POINT ( 'NONE',  ( 52.29715082351538769, 54.60051614449766788, -6.992620115222796251 ) ) ;
#3127 = CARTESIAN_POINT ( 'NONE',  ( 75.00000000000001421, -2.999999999999995559, 10.00000000000000000 ) ) ;
#3128 = AXIS2_PLACEMENT_3D ( 'NONE', #1120, #2707, #13075 ) ;
#3129 = AXIS2_PLACEMENT_3D ( 'NONE', #1340, #7313, #10147 ) ;
#3130 = DIRECTION ( 'NONE',  ( 1.000000000000000000, 0.000000000000000000, 0.000000000000000000 ) ) ;
#3131 = CARTESIAN_POINT ( 'NONE',  ( -4.197312064133472020, -0.8182229787990021874, -3.502518405183886685 ) ) ;
#3132 = ORIENTED_EDGE ( 'NONE', *, *, #19173, .F. ) ;
#3133 =( GEOMETRIC_REPRESENTATION_CONTEXT ( 3 ) GLOBAL_UNCERTAINTY_ASSIGNED_CONTEXT ( ( #15183 ) ) GLOBAL_UNIT_ASSIGNED_CONTEXT ( ( #17088, #6579, #13650 ) ) REPRESENTATION_CONTEXT ( 'NONE', 'WORKASPACE' ) );
#3134 = ORIENTED_EDGE ( 'NONE', *, *, #15693, .T. ) ;
#3135 = VERTEX_POINT ( 'NONE', #7899 ) ;
#3136 = DIRECTION ( 'NONE',  ( -0.000000000000000000, -0.000000000000000000, 1.000000000000000000 ) ) ;
#3137 = CARTESIAN_POINT ( 'NONE',  ( 56.65037692655918988, 47.89948385550240317, -2.184720259617163762 ) ) ;
#3138 = ORIENTED_EDGE ( 'NONE', *, *, #1121, .T. ) ;
#3139 = CARTESIAN_POINT ( 'NONE',  ( 4.898587196589413026E-15, -40.00000000000000000, -9.000000000000000000 ) ) ;
#3140 = CIRCLE ( 'NONE', #16292, 2.649999999999987477 ) ;
#3141 = EDGE_LOOP ( 'NONE', ( #14070, #5455, #11633, #16977 ) ) ;
#3142 = CARTESIAN_POINT ( 'NONE',  ( 56.65037692655921120, 57.10051614449766078, 2.184720259617097593 ) ) ;
#3143 = ORIENTED_EDGE ( 'NONE', *, *, #16372, .T. ) ;
#3144 = FACE_OUTER_BOUND ( 'NONE', #11069, .T. ) ;
#3145 = DIRECTION ( 'NONE',  ( -0.7779254092217071648, -0.6283566325640553840, 0.000000000000000000 ) ) ;
#3146 = AXIS2_PLACEMENT_3D ( 'NONE', #8448, #6484, #611 ) ;
#3147 = CARTESIAN_POINT ( 'NONE',  ( 51.92680522751238925, 53.40051614449765793, 6.007379884777208190 ) ) ;
#3148 = PLANE ( 'NONE',  #16136 ) ;
#3149 = CARTESIAN_POINT ( 'NONE',  ( 50.02271294988511841, 58.49948385550241170, 6.000000000000000888 ) ) ;
#3150 = DIRECTION ( 'NONE',  ( -0.000000000000000000, 1.000000000000000000, -0.000000000000000000 ) ) ;
#3151 = CIRCLE ( 'NONE', #11899, 8.000000000000007105 ) ;
#3152 = CARTESIAN_POINT ( 'NONE',  ( 58.41169779390614281, 51.00051614449765935, 0.02388180880515032231 ) ) ;
#3153 = CARTESIAN_POINT ( 'NONE',  ( 6.327632967270674591, -5.346704644969953790, 0.7392359018479527366 ) ) ;
#3154 = CARTESIAN_POINT ( 'NONE',  ( 4.033901012036086087, 3.740908793663944021, -0.5205559028925770271 ) ) ;
#3155 = AXIS2_PLACEMENT_3D ( 'NONE', #2176, #6298, #18271 ) ;
#3156 = AXIS2_PLACEMENT_3D ( 'NONE', #9071, #10534, #15063 ) ;
#3157 = ORIENTED_EDGE ( 'NONE', *, *, #5919, .T. ) ;
#3158 = CARTESIAN_POINT ( 'NONE',  ( -2.649999999999987477, 15.00000000000001599, 15.00000000000000178 ) ) ;
#3159 = ADVANCED_FACE ( 'NONE', ( #3682 ), #9648, .F. ) ;
#3160 = APPLICATION_PROTOCOL_DEFINITION ( 'draft international standard', 'automotive_design', 1998, #14889 ) ;
#3161 = CIRCLE ( 'NONE', #10321, 4.000000000000003553 ) ;
#3162 = ORIENTED_EDGE ( 'NONE', *, *, #18102, .T. ) ;
#3163 = PRODUCT_RELATED_PRODUCT_CATEGORY ( 'part', '', ( #17289 ) ) ;
#3164 = DIRECTION ( 'NONE',  ( 1.000000000000000000, 0.000000000000000000, 0.000000000000000000 ) ) ;
#3165 = FACE_OUTER_BOUND ( 'NONE', #2916, .T. ) ;
#3166 = AXIS2_PLACEMENT_3D ( 'NONE', #17566, #1371, #12936 ) ;
#3167 = DIRECTION ( 'NONE',  ( 1.000000000000000000, 0.000000000000000000, 0.000000000000000000 ) ) ;
#3168 = CIRCLE ( 'NONE', #16306, 3.799999999999999378 ) ;
#3169 = CARTESIAN_POINT ( 'NONE',  ( 6.436591462021355348, 2.894509378375960118, 5.013437306331775645 ) ) ;
#3170 = AXIS2_PLACEMENT_3D ( 'NONE', #18983, #12788, #8571 ) ;
#3171 = CARTESIAN_POINT ( 'NONE',  ( 6.367873360227556567, 2.886751345948125991, 4.999999999999999112 ) ) ;
#3172 = DIRECTION ( 'NONE',  ( -1.000000000000000000, -0.000000000000000000, -0.000000000000000000 ) ) ;
#3173 = CARTESIAN_POINT ( 'NONE',  ( 55.96859303347804371, 56.19948385550241454, 4.306917132069425946 ) ) ;
#3174 = ADVANCED_FACE ( 'NONE', ( #739 ), #5243, .F. ) ;
#3175 = CARTESIAN_POINT ( 'NONE',  ( 1.249999999999997558, 5.419062086227038392E-16, 4.424999999999999822 ) ) ;
#3176 = CARTESIAN_POINT ( 'NONE',  ( 50.02271294988513972, 56.49948385550240459, 8.000000000000001776 ) ) ;
#3177 = CARTESIAN_POINT ( 'NONE',  ( -74.99999999999997158, -7.499999999999971578, -20.00000000000000000 ) ) ;
#3178 = CARTESIAN_POINT ( 'NONE',  ( 52.29715082351538769, 52.60051614449766788, -6.992620115222796251 ) ) ;
#3179 = CARTESIAN_POINT ( 'NONE',  ( 5.130877905917420101, -39.33065161639846252, 0.000000000000000000 ) ) ;
#3180 = CIRCLE ( 'NONE', #1607, 5.999999999999977796 ) ;
#3181 = EDGE_CURVE ( 'NONE', #1266, #14141, #11772, .T. ) ;
#3182 = ADVANCED_FACE ( 'NONE', ( #6908 ), #13275, .F. ) ;
#3183 = AXIS2_PLACEMENT_3D ( 'NONE', #15961, #8694, #7029 ) ;
#3184 = ORIENTED_EDGE ( 'NONE', *, *, #1535, .F. ) ;
#3185 = CARTESIAN_POINT ( 'NONE',  ( 4.211140560182196957, 2.431303136016536470, -3.745885042887433514 ) ) ;
#3186 = ORIENTED_EDGE ( 'NONE', *, *, #669, .F. ) ;
#3187 = DIRECTION ( 'NONE',  ( -0.000000000000000000, -0.000000000000000000, 1.000000000000000000 ) ) ;
#3188 = ADVANCED_FACE ( 'NONE', ( #2804 ), #14830, .T. ) ;
#3189 = CARTESIAN_POINT ( 'NONE',  ( -17.32050807568872841, -30.00000000000008171, -9.000000000000000000 ) ) ;
#3190 = CARTESIAN_POINT ( 'NONE',  ( -154.8505191518487152, -18.79705879280739467, -15.79999999999999893 ) ) ;
#3191 = ORIENTED_EDGE ( 'NONE', *, *, #7720, .F. ) ;
#3192 = CARTESIAN_POINT ( 'NONE',  ( -62.49999999999997158, 45.00000000000001421, 15.00000000000000000 ) ) ;
#3193 = LINE ( 'NONE', #5830, #8882 ) ;
#3194 = CARTESIAN_POINT ( 'NONE',  ( 56.30877334542961421, 57.99948385550241170, -0.02388180880520959434 ) ) ;
#3195 = FACE_OUTER_BOUND ( 'NONE', #4798, .T. ) ;
#3196 = AXIS2_PLACEMENT_3D ( 'NONE', #10224, #4259, #4072 ) ;
#3197 = VECTOR ( 'NONE', #1402, 1000.000000000000000 ) ;
#3198 = CARTESIAN_POINT ( 'NONE',  ( 50.02271294988505446, 50.50051614449765935, -8.000000000000001776 ) ) ;
#3199 = CARTESIAN_POINT ( 'NONE',  ( 50.02271294988506156, 56.50051614449767357, -6.000000000000000888 ) ) ;
#3200 = VECTOR ( 'NONE', #2745, 1000.000000000000000 ) ;
#3201 = DIRECTION ( 'NONE',  ( 1.000000000000000000, 0.000000000000000000, 0.000000000000000000 ) ) ;
#3202 = CARTESIAN_POINT ( 'NONE',  ( 6.506891779418576327, -2.833891091414761032, -5.091556646552826138 ) ) ;
#3204 = ORIENTED_EDGE ( 'NONE', *, *, #4625, .F. ) ;
#3203 = ADVANCED_FACE ( 'NONE', ( #5736 ), #17617, .T. ) ;
#3205 = EDGE_CURVE ( 'NONE', #14054, #15034, #6646, .T. ) ;
#3206 = VERTEX_POINT ( 'NONE', #10134 ) ;
#3207 = CARTESIAN_POINT ( 'NONE',  ( 6.242811304425483598, -0.9953138271174254426, -5.105233480330447549 ) ) ;
#3208 = EDGE_LOOP ( 'NONE', ( #4399, #3539, #9450, #15588 ) ) ;
#3209 = CARTESIAN_POINT ( 'NONE',  ( 55.94051828345050836, 63.79948385550240886, -4.345558710429104465 ) ) ;
#3210 = CARTESIAN_POINT ( 'NONE',  ( -1.150000000000000577, 0.000000000000000000, 0.000000000000000000 ) ) ;
#3211 = EDGE_LOOP ( 'NONE', ( #15466, #11129, #3893, #3157 ) ) ;
#3212 = PLANE ( 'NONE',  #13485 ) ;
#3213 = CARTESIAN_POINT ( 'NONE',  ( 49.97728705011488159, 49.49948385550240459, -7.000000000000000888 ) ) ;
#3214 = VERTEX_POINT ( 'NONE', #7301 ) ;
#3215 = CARTESIAN_POINT ( 'NONE',  ( 0.000000000000000000, -0.8865213383406694847, 1.535500000000001419 ) ) ;
#3216 = EDGE_LOOP ( 'NONE', ( #1434, #10455, #45, #10225, #9864, #15578, #757, #12437 ) ) ;
#3217 = CARTESIAN_POINT ( 'NONE',  ( 56.79116909180259398, 63.20051614449766220, 4.963592699178938972 ) ) ;
#3218 = DIRECTION ( 'NONE',  ( 0.000000000000000000, -0.000000000000000000, 1.000000000000000000 ) ) ;
#3219 = CARTESIAN_POINT ( 'NONE',  ( 52.29715082351547295, 56.39948385550238896, 6.992620115222774047 ) ) ;
#3220 = CARTESIAN_POINT ( 'NONE',  ( -154.8505191518487152, -18.79705879280739467, -15.79999999999999893 ) ) ;
#3221 = CARTESIAN_POINT ( 'NONE',  ( 45.86712807150329496, 51.70051614449766220, 5.649768623646139964 ) ) ;
#3222 = EDGE_CURVE ( 'NONE', #206, #18916, #17044, .T. ) ;
#3223 = CARTESIAN_POINT ( 'NONE',  ( 5.991014884144048480, -4.770489558936219510E-15, -5.000000000000000000 ) ) ;
#3224 = AXIS2_PLACEMENT_3D ( 'NONE', #16140, #8671, #14643 ) ;
#3225 = CARTESIAN_POINT ( 'NONE',  ( -74.99999999999997158, -1.000000000000000000, -5.999999999999998224 ) ) ;
#3226 = ORIENTED_EDGE ( 'NONE', *, *, #14676, .F. ) ;
#3227 = ADVANCED_FACE ( 'NONE', ( #19092 ), #5347, .T. ) ;
#3228 = VERTEX_POINT ( 'NONE', #7099 ) ;
#3229 = ORIENTED_EDGE ( 'NONE', *, *, #17743, .F. ) ;
#3230 = LINE ( 'NONE', #11037, #3408 ) ;
#3231 = CARTESIAN_POINT ( 'NONE',  ( 56.79116909180255135, 63.79948385550241596, -4.963592699179005585 ) ) ;
#3232 = DIRECTION ( 'NONE',  ( -0.000000000000000000, -0.000000000000000000, 1.000000000000000000 ) ) ;
#3233 = ORIENTED_EDGE ( 'NONE', *, *, #9384, .T. ) ;
#3234 = DIRECTION ( 'NONE',  ( 0.000000000000000000, 0.000000000000000000, 1.000000000000000000 ) ) ;
#3235 = VERTEX_POINT ( 'NONE', #16137 ) ;
#3236 = CARTESIAN_POINT ( 'NONE',  ( 44.03140696652198471, 57.80051614449766362, 4.306917132069485454 ) ) ;
#3237 = ORIENTED_EDGE ( 'NONE', *, *, #16836, .F. ) ;
#3238 = CARTESIAN_POINT ( 'NONE',  ( 6.244004651191001010, -4.178905357954647570, 2.972460101650454600 ) ) ;
#3239 = UNCERTAINTY_MEASURE_WITH_UNIT (LENGTH_MEASURE( 1.000000000000000082E-05 ), #11941, 'distance_accuracy_value', 'NONE');
#3240 = LINE ( 'NONE', #12050, #13687 ) ;
#3241 = AXIS2_PLACEMENT_3D ( 'NONE', #13242, #2873, #2772 ) ;
#3242 = CARTESIAN_POINT ( 'NONE',  ( 44.88205777487401349, 57.80051614449766362, 3.688883143319584779 ) ) ;
#3243 = DIRECTION ( 'NONE',  ( -0.7779254092217071648, -0.6283566325640553840, 1.130512422757410748E-16 ) ) ;
#3244 = EDGE_CURVE ( 'NONE', #16758, #5231, #4518, .T. ) ;
#3245 = CARTESIAN_POINT ( 'NONE',  ( -74.99999999999997158, 40.00000000000001421, 10.00000000000000000 ) ) ;
#3246 = CARTESIAN_POINT ( 'NONE',  ( 55.69932041026404335, 59.89948385550240317, -1.875703265242203432 ) ) ;
#3247 = CARTESIAN_POINT ( 'NONE',  ( 0.5469614295415388128, -4.303013824935362663, -3.535263753543555598 ) ) ;
#3248 = CARTESIAN_POINT ( 'NONE',  ( 49.97728705011495265, 55.50051614449766646, 8.000000000000001776 ) ) ;
#3249 = DIRECTION ( 'NONE',  ( 0.000000000000000000, 0.000000000000000000, 1.000000000000000000 ) ) ;
#3250 = ORIENTED_EDGE ( 'NONE', *, *, #10236, .F. ) ;
#3251 = DIRECTION ( 'NONE',  ( -0.000000000000000000, -0.000000000000000000, -1.000000000000000000 ) ) ;
#3252 = CARTESIAN_POINT ( 'NONE',  ( -18.89043790736545603, -22.09056926535314602, -9.000000000000000000 ) ) ;
#3253 = PRODUCT_CONTEXT ( 'NONE', #2406, 'mechanical' ) ;
#3254 = VERTEX_POINT ( 'NONE', #9838 ) ;
#3255 = CYLINDRICAL_SURFACE ( 'NONE', #11433, 0.7500000000000002220 ) ;
#3256 = CARTESIAN_POINT ( 'NONE',  ( 62.49999999999998579, 40.00000000000001421, 9.999999999999998224 ) ) ;
#3257 = CARTESIAN_POINT ( 'NONE',  ( 47.70284917648453415, 61.39948385550241028, -6.992620115222774047 ) ) ;
#3258 = DIRECTION ( 'NONE',  ( 1.000000000000000000, 0.000000000000000000, 0.000000000000000000 ) ) ;
#3259 = CARTESIAN_POINT ( 'NONE',  ( 17.79870116617236420, -10.87825472854593301, -9.000000000000000000 ) ) ;
#3260 = DIRECTION ( 'NONE',  ( 1.000000000000000000, 0.000000000000000000, 0.000000000000000000 ) ) ;
#3261 = CARTESIAN_POINT ( 'NONE',  ( 52.25172492374522903, 61.59948385550239891, -7.007379884777225953 ) ) ;
#3262 = DIRECTION ( 'NONE',  ( -0.000000000000000000, -0.000000000000000000, 1.000000000000000000 ) ) ;
#3263 = CARTESIAN_POINT ( 'NONE',  ( 43.20883090819745576, 58.79948385550240175, 4.963592699179006473 ) ) ;
#3264 = CARTESIAN_POINT ( 'NONE',  ( 43.34962307344078880, 56.10051614449766078, -2.184720259617096705 ) ) ;
#3265 = CYLINDRICAL_SURFACE ( 'NONE', #4737, 1.000000000000000000 ) ;
#3266 = ORIENTED_EDGE ( 'NONE', *, *, #10585, .F. ) ;
#3267 = VECTOR ( 'NONE', #14034, 1000.000000000000000 ) ;
#3268 = CARTESIAN_POINT ( 'NONE',  ( 4.197393957002303999, 0.8151795401431359833, -3.503767560748935139 ) ) ;
#3269 = CARTESIAN_POINT ( 'NONE',  ( 45.86712807150329496, 45.70051614449766220, 5.649768623646139964 ) ) ;
#3270 = CARTESIAN_POINT ( 'NONE',  ( 44.05948171654949874, 64.79948385550240175, 4.345558710429105354 ) ) ;
#3271 = CARTESIAN_POINT ( 'NONE',  ( -32.00000000000000000, 1.000000000000000000, 6.000000000000000000 ) ) ;
#3272 = ORIENTED_EDGE ( 'NONE', *, *, #10957, .T. ) ;
#3273 = CYLINDRICAL_SURFACE ( 'NONE', #15867, 1.000000000000000000 ) ;
#3274 = DIRECTION ( 'NONE',  ( -1.000000000000000000, 0.000000000000000000, 0.000000000000000000 ) ) ;
#3275 = EDGE_CURVE ( 'NONE', #3719, #8297, #11699, .T. ) ;
#3276 = CARTESIAN_POINT ( 'NONE',  ( 56.30877334542961421, 45.00051614449765225, 0.02388180880515774693 ) ) ;
#3277 = CYLINDRICAL_SURFACE ( 'NONE', #18570, 1.000000000000000888 ) ;
#3278 = CARTESIAN_POINT ( 'NONE',  ( 17.85000000000000142, -20.00000000000000000, -20.00000000000000000 ) ) ;
#3279 = CARTESIAN_POINT ( 'NONE',  ( 47.42335538002180328, 52.40051614449767214, -8.007379884777206414 ) ) ;
#3280 = CIRCLE ( 'NONE', #14528, 3.500000000000000000 ) ;
#3281 = PRODUCT_DEFINITION ( 'UNKNOWN', '', #14811, #18341 ) ;
#3282 = CARTESIAN_POINT ( 'NONE',  ( 51.92680522751238925, 53.40051614449765793, 6.007379884777208190 ) ) ;
#3283 = EDGE_CURVE ( 'NONE', #5389, #16193, #2525, .T. ) ;
#3284 = CARTESIAN_POINT ( 'NONE',  ( -4.211140560182196957, -2.431303136016552013, -3.745885042887436178 ) ) ;
#3285 = DIRECTION ( 'NONE',  ( -1.000000000000000000, 0.000000000000000000, -0.000000000000000000 ) ) ;
#3286 = AXIS2_PLACEMENT_3D ( 'NONE', #5019, #15506, #11084 ) ;
#3287 = ORIENTED_EDGE ( 'NONE', *, *, #17366, .T. ) ;
#3288 = ADVANCED_FACE ( 'NONE', ( #2715 ), #17355, .F. ) ;
#3289 = EDGE_CURVE ( 'NONE', #14650, #3573, #19196, .T. ) ;
#3290 = ORIENTED_EDGE ( 'NONE', *, *, #9510, .F. ) ;
#3291 = CARTESIAN_POINT ( 'NONE',  ( 6.390983168987730778, -3.014662706507984513, -5.000000000000000000 ) ) ;
#3292 = EDGE_LOOP ( 'NONE', ( #10273, #10369, #13678, #17207 ) ) ;
#3293 = EDGE_CURVE ( 'NONE', #13672, #1920, #12983, .T. ) ;
#3294 = CARTESIAN_POINT ( 'NONE',  ( 32.49999999999998579, 5.000000000000018652, 5.000000000000003553 ) ) ;
#3295 = AXIS2_PLACEMENT_3D ( 'NONE', #16109, #6193, #5104 ) ;
#3296 =( BOUNDED_SURFACE ( )  B_SPLINE_SURFACE ( 3, 2, ( 
 ( #11832, #13307, #13511 ),
 ( #1659, #19324, #11733 ),
 ( #4295, #5863, #7622 ),
 ( #17837, #17941, #3131 ),
 ( #4592, #4398, #10365 ),
 ( #19227, #8989, #6150 ) ),
 .UNSPECIFIED., .F., .F., .F. ) 
 B_SPLINE_SURFACE_WITH_KNOTS ( ( 4, 2, 4 ),
 ( 3, 3 ),
 ( 0.02027752710269158445, 0.02273781595091097299, 0.02519810479913036153 ),
 ( 0.000000000000000000, 1.000000000000000000 ),
 .UNSPECIFIED. ) 
 GEOMETRIC_REPRESENTATION_ITEM ( )  RATIONAL_B_SPLINE_SURFACE ( (
 ( 1.000000000000000000, 0.8047781431712808242, 1.000000000000000000),
 ( 1.000000000000000000, 0.8123773247083928561, 1.000000000000000000),
 ( 1.000000000000000000, 0.8190670192154906326, 1.000000000000000000),
 ( 1.000000000000000000, 0.8192353552912178261, 1.000000000000000000),
 ( 1.000000000000000000, 0.8126132098226825917, 1.000000000000000000),
 ( 1.000000000000000000, 0.8047712465856394770, 1.000000000000000000) ) ) 
 REPRESENTATION_ITEM ( '' )  SURFACE ( )  );
#3297 = VERTEX_POINT ( 'NONE', #14640 ) ;
#3298 = VECTOR ( 'NONE', #3815, 1000.000000000000114 ) ;
#3299 = CARTESIAN_POINT ( 'NONE',  ( 2.449293598294706513E-15, -20.00000000000000000, -23.00000000000000000 ) ) ;
#3300 = CARTESIAN_POINT ( 'NONE',  ( 57.36023556966787851, 49.99948385550239749, -0.02388180880522424582 ) ) ;
#3301 = EDGE_LOOP ( 'NONE', ( #9682, #10312, #5828, #1389, #4811 ) ) ;
#3302 = PLANE ( 'NONE',  #15384 ) ;
#3303 = ORIENTED_EDGE ( 'NONE', *, *, #295, .T. ) ;
#3304 = CARTESIAN_POINT ( 'NONE',  ( 50.02271294988513972, 48.49948385550241170, 8.000000000000001776 ) ) ;
#3305 = CYLINDRICAL_SURFACE ( 'NONE', #1949, 6.000000000000001776 ) ;
#3306 = VECTOR ( 'NONE', #403, 1000.000000000000000 ) ;
#3307 = EDGE_CURVE ( 'NONE', #5263, #6112, #12645, .T. ) ;
#3308 = CARTESIAN_POINT ( 'NONE',  ( 56.66441430157296821, 58.09948385550240602, 2.141517661632100111 ) ) ;
#3309 = CARTESIAN_POINT ( 'NONE',  ( 2.141980652367355464, -6.189445006155633422, -0.8000000000000000444 ) ) ;
#3310 = ADVANCED_FACE ( 'NONE', ( #17904, #16624 ), #18096, .F. ) ;
#3311 = CARTESIAN_POINT ( 'NONE',  ( -44.99999999999997158, -7.499999999999971578, -10.00000000000000000 ) ) ;
#3312 = CARTESIAN_POINT ( 'NONE',  ( 54.09612160359792199, 53.30051614449766362, 5.676469297603124353 ) ) ;
#3313 = CARTESIAN_POINT ( 'NONE',  ( -155.0777214229742071, -18.79920509849242549, 15.00000000000000000 ) ) ;
#3314 = CARTESIAN_POINT ( 'NONE',  ( 45.90387839640214196, 52.69948385550240033, 5.676469297603166098 ) ) ;
#3315 = DIRECTION ( 'NONE',  ( 0.000000000000000000, 0.000000000000000000, 1.000000000000000000 ) ) ;
#3316 = VERTEX_POINT ( 'NONE', #7586 ) ;
#3317 = B_SPLINE_CURVE_WITH_KNOTS ( 'NONE', 3,
 ( #11518, #17527, #4088, #15554 ),
 .UNSPECIFIED., .F., .F.,
 ( 4, 4 ),
 ( 2.380739282167303683E-07, 0.002044882221487525839 ),
 .UNSPECIFIED. ) ;
#3318 = ORIENTED_EDGE ( 'NONE', *, *, #15393, .T. ) ;
#3319 = ORIENTED_EDGE ( 'NONE', *, *, #1535, .T. ) ;
#3320 = CIRCLE ( 'NONE', #1129, 1.000000000000001110 ) ;
#3321 = CARTESIAN_POINT ( 'NONE',  ( 43.33558569842703179, 55.09948385550241312, -2.141517661632099223 ) ) ;
#3322 = LINE ( 'NONE', #3602, #15614 ) ;
#3323 = ORIENTED_EDGE ( 'NONE', *, *, #17364, .T. ) ;
#3324 = CARTESIAN_POINT ( 'NONE',  ( 6.534838248920899595, 5.903531555104835071, 8.098083288904839678E-18 ) ) ;
#3325 = AXIS2_PLACEMENT_3D ( 'NONE', #14873, #8803, #1355 ) ;
#3326 = VERTEX_POINT ( 'NONE', #11798 ) ;
#3327 = CARTESIAN_POINT ( 'NONE',  ( 50.02271294988505446, 58.50051614449765935, -7.000000000000000888 ) ) ;
#3328 = ORIENTED_EDGE ( 'NONE', *, *, #12262, .F. ) ;
#3329 = LINE ( 'NONE', #1671, #7222 ) ;
#3330 = DIRECTION ( 'NONE',  ( 1.000000000000000000, -0.000000000000000000, -0.000000000000000000 ) ) ;
#3331 = CARTESIAN_POINT ( 'NONE',  ( 48.07319477248762496, 58.40051614449765793, -6.007379884777208190 ) ) ;
#3332 = DIRECTION ( 'NONE',  ( -1.000000000000000000, -3.469446951953615175E-16, 0.000000000000000000 ) ) ;
#3333 = AXIS2_PLACEMENT_3D ( 'NONE', #14589, #19138, #8816 ) ;
#3334 = CARTESIAN_POINT ( 'NONE',  ( 0.1996310553826632361, 1.947030205581113282, 4.999999999999997335 ) ) ;
#3335 = ADVANCED_FACE ( 'NONE', ( #10518, #1519 ), #6032, .T. ) ;
#3336 = CARTESIAN_POINT ( 'NONE',  ( 55.71335778527780747, 62.09948385550240602, 1.832500667257165983 ) ) ;
#3337 = DIRECTION ( 'NONE',  ( -0.000000000000000000, -0.000000000000000000, 1.000000000000000000 ) ) ;
#3338 = CARTESIAN_POINT ( 'NONE',  ( 42.38452918213190657, 61.90051614449766504, 2.450534656007115508 ) ) ;
#3339 = VERTEX_POINT ( 'NONE', #2903 ) ;
#3340 = CARTESIAN_POINT ( 'NONE',  ( -54.99999999999996447, -6.999999999999985789, 15.00000000000000000 ) ) ;
#3341 = SHAPE_REPRESENTATION_RELATIONSHIP ( 'NONE' , 'NONE' ,  #4676, #16200 ) ;
#3342 = ORIENTED_EDGE ( 'NONE', *, *, #17496, .T. ) ;
#3343 =( NAMED_UNIT ( * ) PLANE_ANGLE_UNIT ( ) SI_UNIT ( $, .RADIAN. ) );
#3344 = APPLICATION_PROTOCOL_DEFINITION ( 'draft international standard', 'automotive_design', 1998, #11656 ) ;
#3345 = ORIENTED_EDGE ( 'NONE', *, *, #9091, .T. ) ;
#3346 = AXIS2_PLACEMENT_3D ( 'NONE', #614, #7962, #15717 ) ;
#3347 = CARTESIAN_POINT ( 'NONE',  ( -22.00000000000000000, -19.99999999999999289, -20.00000000000000000 ) ) ;
#3348 = EDGE_CURVE ( 'NONE', #7873, #4201, #3193, .T. ) ;
#3349 = LINE ( 'NONE', #4908, #16918 ) ;
#3350 = EDGE_CURVE ( 'NONE', #3064, #12768, #1808, .T. ) ;
#3351 = CARTESIAN_POINT ( 'NONE',  ( 52.25172492374522903, 63.59948385550239180, -7.007379884777227730 ) ) ;
#3352 = CARTESIAN_POINT ( 'NONE',  ( -32.00000000000000000, -3.000000000000000000, 6.000000000000001776 ) ) ;
#3353 = FACE_OUTER_BOUND ( 'NONE', #13021, .T. ) ;
#3354 = CIRCLE ( 'NONE', #529, 4.424999999999999822 ) ;
#3355 = DIRECTION ( 'NONE',  ( 0.000000000000000000, 0.000000000000000000, -1.000000000000000000 ) ) ;
#3356 = CARTESIAN_POINT ( 'NONE',  ( 48.02776887271745210, 47.39948385550241028, -5.992620115222778487 ) ) ;
#3357 = CARTESIAN_POINT ( 'NONE',  ( -154.9999999999999716, -14.99999999999999645, 4.000000000000000000 ) ) ;
#3358 = CARTESIAN_POINT ( 'NONE',  ( 56.79116909180255135, 61.79948385550240175, -4.963592699179005585 ) ) ;
#3359 = CARTESIAN_POINT ( 'NONE',  ( 55.94051828345053679, 57.20051614449766930, 4.345558710429044069 ) ) ;
#3360 = FACE_OUTER_BOUND ( 'NONE', #8105, .T. ) ;
#3361 = LINE ( 'NONE', #3179, #5338 ) ;
#3362 = VERTEX_POINT ( 'NONE', #10425 ) ;
#3363 = AXIS2_PLACEMENT_3D ( 'NONE', #11287, #9717, #17294 ) ;
#3364 = CARTESIAN_POINT ( 'NONE',  ( 6.506987859255528583, 2.925375531177297095, -5.066899051217877314 ) ) ;
#3365 = CIRCLE ( 'NONE', #1492, 20.00000000000000000 ) ;
#3366 = CARTESIAN_POINT ( 'NONE',  ( -158.9999999999999716, -14.99999999999999645, 15.00000000000000000 ) ) ;
#3367 = CARTESIAN_POINT ( 'NONE',  ( 56.65037692655918988, 61.89948385550241028, -2.184720259617163762 ) ) ;
#3368 = DIRECTION ( 'NONE',  ( -0.7071067811865350272, 8.659560562355083235E-17, -0.7071067811865598962 ) ) ;
#3369 = ORIENTED_EDGE ( 'NONE', *, *, #14240, .T. ) ;
#3370 = FACE_OUTER_BOUND ( 'NONE', #18818, .T. ) ;
#3371 = FACE_OUTER_BOUND ( 'NONE', #18136, .T. ) ;
#3372 = CARTESIAN_POINT ( 'NONE',  ( 55.08986747509847248, 63.79948385550241596, -3.727524721679197572 ) ) ;
#3373 = DIRECTION ( 'NONE',  ( -0.000000000000000000, -1.000000000000000000, -0.000000000000000000 ) ) ;
#3374 = CARTESIAN_POINT ( 'NONE',  ( 0.3117969352650132309, 2.419842229202153305, -4.999999999999999112 ) ) ;
#3375 = CIRCLE ( 'NONE', #14317, 2.000000000000000000 ) ;
#3376 = CARTESIAN_POINT ( 'NONE',  ( 57.61547081786810764, 58.90051614449766504, -2.450534656007114176 ) ) ;
#3377 = CARTESIAN_POINT ( 'NONE',  ( 55.69932041026405045, 57.10051614449766788, 1.875703265242156359 ) ) ;
#3378 = AXIS2_PLACEMENT_3D ( 'NONE', #5893, #11859, #8924 ) ;
#3379 = CARTESIAN_POINT ( 'NONE',  ( -20.63749999999999574, 0.000000000000000000, 0.000000000000000000 ) ) ;
#3380 = VECTOR ( 'NONE', #10522, 1000.000000000000000 ) ;
#3381 = FACE_OUTER_BOUND ( 'NONE', #7891, .T. ) ;
#3382 = ORIENTED_EDGE ( 'NONE', *, *, #3042, .T. ) ;
#3383 = ORIENTED_EDGE ( 'NONE', *, *, #748, .T. ) ;
#3384 = ORIENTED_EDGE ( 'NONE', *, *, #9540, .T. ) ;
#3385 = EDGE_CURVE ( 'NONE', #4604, #1126, #13262, .T. ) ;
#3386 = DIRECTION ( 'NONE',  ( -0.000000000000000000, -0.000000000000000000, 1.000000000000000000 ) ) ;
#3387 = B_SPLINE_CURVE_WITH_KNOTS ( 'NONE', 3,
 ( #5744, #14854, #8680, #3105, #13381 ),
 .UNSPECIFIED., .F., .F.,
 ( 4, 1, 4 ),
 ( 0.000000000000000000, 0.002309401076758506657, 0.004618802153517013315 ),
 .UNSPECIFIED. ) ;
#3388 = ORIENTED_EDGE ( 'NONE', *, *, #9768, .F. ) ;
#3389 = CARTESIAN_POINT ( 'NONE',  ( 75.00000000000001421, 3.000000000000002665, 10.00000000000000000 ) ) ;
#3390 = CIRCLE ( 'NONE', #269, 2.000000000000001776 ) ;
#3391 = CARTESIAN_POINT ( 'NONE',  ( 50.02271294988512551, 52.49948385550240459, 7.000000000000000888 ) ) ;
#3392 = AXIS2_PLACEMENT_3D ( 'NONE', #17067, #18553, #14097 ) ;
#3393 = VERTEX_POINT ( 'NONE', #6121 ) ;
#3394 = DIRECTION ( 'NONE',  ( 0.000000000000000000, 0.000000000000000000, 1.000000000000000000 ) ) ;
#3395 = EDGE_LOOP ( 'NONE', ( #543, #12816, #15148, #9107 ) ) ;
#3396 = CARTESIAN_POINT ( 'NONE',  ( 47.37792948025162332, 49.39948385550241028, -7.992620115222770494 ) ) ;
#3397 = LINE ( 'NONE', #2028, #17988 ) ;
#3398 = CARTESIAN_POINT ( 'NONE',  ( 56.30877334542961421, 45.99948385550240459, -0.02388180880520959434 ) ) ;
#3399 = CARTESIAN_POINT ( 'NONE',  ( 4.180345304246197990, 4.135116856707394817, -0.02129519942689619277 ) ) ;
#3400 = CARTESIAN_POINT ( 'NONE',  ( 9.037824375505689289, -37.84146099840243949, -9.000000000000000000 ) ) ;
#3401 =( GEOMETRIC_REPRESENTATION_CONTEXT ( 3 ) GLOBAL_UNCERTAINTY_ASSIGNED_CONTEXT ( ( #4982 ) ) GLOBAL_UNIT_ASSIGNED_CONTEXT ( ( #9123, #1586, #113 ) ) REPRESENTATION_CONTEXT ( 'NONE', 'WORKASPACE' ) );
#3402 = CARTESIAN_POINT ( 'NONE',  ( 57.36023556966787851, 63.00051614449767357, 0.02388180880515038476 ) ) ;
#3403 = FACE_OUTER_BOUND ( 'NONE', #11668, .T. ) ;
#3404 = EDGE_CURVE ( 'NONE', #19012, #11405, #2323, .T. ) ;
#3405 = CARTESIAN_POINT ( 'NONE',  ( 54.13287192849676188, 52.29948385550240886, 5.649768623646098220 ) ) ;
#3406 = CARTESIAN_POINT ( 'NONE',  ( 6.527192678185836705, -5.883244248022288403, -1.193258867985458992E-13 ) ) ;
#3407 = VECTOR ( 'NONE', #11356, 1000.000000000000000 ) ;
#3408 = VECTOR ( 'NONE', #7814, 1000.000000000000000 ) ;
#3410 = VERTEX_POINT ( 'NONE', #9155 ) ;
#3409 =( BOUNDED_SURFACE ( )  B_SPLINE_SURFACE ( 3, 2, ( 
 ( #11218, #6715, #11321 ),
 ( #17224, #11121, #7902 ),
 ( #3685, #9752, #2123 ),
 ( #5057, #18608, #14158 ),
 ( #2324, #8277, #12801 ),
 ( #15449, #9463, #3399 ) ),
 .UNSPECIFIED., .F., .F., .F. ) 
 B_SPLINE_SURFACE_WITH_KNOTS ( ( 4, 2, 4 ),
 ( 3, 3 ),
 ( 0.01651999345535505245, 0.01858032176739834312, 0.02064065007944163727 ),
 ( 0.000000000000000000, 1.000000000000000000 ),
 .UNSPECIFIED. ) 
 GEOMETRIC_REPRESENTATION_ITEM ( )  RATIONAL_B_SPLINE_SURFACE ( (
 ( 1.000000000000000000, 0.8047781103519393575, 1.000000000000000000),
 ( 1.000000000000000000, 0.8123785825604844524, 1.000000000000000000),
 ( 1.000000000000000000, 0.8190671539787625077, 1.000000000000000000),
 ( 1.000000000000000000, 0.8192352254835536529, 1.000000000000000000),
 ( 1.000000000000000000, 0.8126129677211098024, 1.000000000000000000),
 ( 1.000000000000000000, 0.8047712537969730073, 1.000000000000000000) ) ) 
 REPRESENTATION_ITEM ( '' )  SURFACE ( )  );
#3411 = ORIENTED_EDGE ( 'NONE', *, *, #15144, .T. ) ;
#3412 = CARTESIAN_POINT ( 'NONE',  ( -54.99999999999996447, -6.999999999999985789, -15.00000000000000000 ) ) ;
#3413 = EDGE_CURVE ( 'NONE', #14560, #8619, #2995, .T. ) ;
#3414 = CARTESIAN_POINT ( 'NONE',  ( 49.97728705011488159, 49.49948385550240459, -7.000000000000000888 ) ) ;
#3415 = EDGE_CURVE ( 'NONE', #2892, #8396, #17999, .T. ) ;
#3416 =( GEOMETRIC_REPRESENTATION_CONTEXT ( 3 ) GLOBAL_UNCERTAINTY_ASSIGNED_CONTEXT ( ( #11848 ) ) GLOBAL_UNIT_ASSIGNED_CONTEXT ( ( #9563, #12709, #12611 ) ) REPRESENTATION_CONTEXT ( 'NONE', 'WORKASPACE' ) );
#3417 = ORIENTED_EDGE ( 'NONE', *, *, #11894, .F. ) ;
#3418 = DIRECTION ( 'NONE',  ( 1.000000000000000000, 0.000000000000000000, 0.000000000000000000 ) ) ;
#3419 = EDGE_LOOP ( 'NONE', ( #18617, #9090 ) ) ;
#3420 = DIRECTION ( 'NONE',  ( 1.000000000000000000, 0.000000000000000000, 0.000000000000000000 ) ) ;
#3421 = ORIENTED_EDGE ( 'NONE', *, *, #18544, .F. ) ;
#3422 = AXIS2_PLACEMENT_3D ( 'NONE', #664, #16952, #15176 ) ;
#3423 = EDGE_CURVE ( 'NONE', #3696, #8654, #18928, .T. ) ;
#3424 = CIRCLE ( 'NONE', #2180, 1.000000000000000222 ) ;
#3425 = CARTESIAN_POINT ( 'NONE',  ( -19.30627432446643610, -25.22185519795866782, 0.000000000000000000 ) ) ;
#3426 = UNCERTAINTY_MEASURE_WITH_UNIT (LENGTH_MEASURE( 1.000000000000000082E-05 ), #5894, 'distance_accuracy_value', 'NONE');
#3427 = CARTESIAN_POINT ( 'NONE',  ( -7.211304515372694901, -1.345319965580611843, 0.000000000000000000 ) ) ;
#3428 = ADVANCED_FACE ( 'NONE', ( #16330 ), #15133, .T. ) ;
#3429 = CARTESIAN_POINT ( 'NONE',  ( 44.30067958973594955, 56.10051614449766078, -1.875703265242155693 ) ) ;
#3430 = PLANE ( 'NONE',  #8912 ) ;
#3431 = ADVANCED_FACE ( 'NONE', ( #14843 ), #7679, .T. ) ;
#3432 = CARTESIAN_POINT ( 'NONE',  ( -1.000000000000000222, -4.808326913195983821, -0.8000000000000000444 ) ) ;
#3433 = AXIS2_PLACEMENT_3D ( 'NONE', #898, #6679, #17584 ) ;
#3434 = CARTESIAN_POINT ( 'NONE',  ( -3.799999999999999378, 4.653657836759941744E-16, 0.000000000000000000 ) ) ;
#3435 = CARTESIAN_POINT ( 'NONE',  ( 47.42335538002180328, 62.40051614449765793, -8.007379884777206414 ) ) ;
#3436 = ORIENTED_EDGE ( 'NONE', *, *, #423, .F. ) ;
#3437 = ORIENTED_EDGE ( 'NONE', *, *, #2137, .T. ) ;
#3438 = DIRECTION ( 'NONE',  ( 1.000000000000000000, 0.000000000000000000, 0.000000000000000000 ) ) ;
#3439 = SURFACE_SIDE_STYLE ('',( #16874 ) ) ;
#3440 = AXIS2_PLACEMENT_3D ( 'NONE', #156, #12393, #3488 ) ;
#3441 = ORIENTED_EDGE ( 'NONE', *, *, #6041, .T. ) ;
#3442 = CIRCLE ( 'NONE', #15964, 20.00000000000000000 ) ;
#3443 = CONTEXT_DEPENDENT_SHAPE_REPRESENTATION ( #15302, #5867 ) ;
#3444 = ORIENTED_EDGE ( 'NONE', *, *, #9373, .F. ) ;
#3445 = CARTESIAN_POINT ( 'NONE',  ( 1.250000000000001110, 0.000000000000000000, 0.000000000000000000 ) ) ;
#3446 = LINE ( 'NONE', #1974, #8446 ) ;
#3447 = VECTOR ( 'NONE', #15223, 1000.000000000000000 ) ;
#3448 = CARTESIAN_POINT ( 'NONE',  ( -154.9999999999999716, -14.99999999999999645, -10.00000000000000000 ) ) ;
#3449 = DIRECTION ( 'NONE',  ( 1.000000000000000000, 0.000000000000000000, 0.000000000000000000 ) ) ;
#3450 = VECTOR ( 'NONE', #6682, 1000.000000000000000 ) ;
#3451 = LINE ( 'NONE', #7942, #3901 ) ;
#3452 = DIRECTION ( 'NONE',  ( 0.000000000000000000, 0.000000000000000000, 1.000000000000000000 ) ) ;
#3453 = CARTESIAN_POINT ( 'NONE',  ( 56.66441430157296821, 64.09948385550239891, 2.141517661632100111 ) ) ;
#3454 = CARTESIAN_POINT ( 'NONE',  ( 50.00000000000000000, 40.00000000000000000, -4.000000000000003553 ) ) ;
#3455 = CARTESIAN_POINT ( 'NONE',  ( 45.27934281921075410, 57.29948385550240175, -6.458785618021043895 ) ) ;
#3456 = CARTESIAN_POINT ( 'NONE',  ( 49.97728705011495265, 61.50051614449765935, 7.000000000000000888 ) ) ;
#3457 = EDGE_CURVE ( 'NONE', #12327, #8171, #7006, .T. ) ;
#3458 = CIRCLE ( 'NONE', #17, 6.000000000000000888 ) ;
#3459 = CARTESIAN_POINT ( 'NONE',  ( 0.000000000000000000, 0.000000000000000000, -1.000000000000000000 ) ) ;
#3460 = CARTESIAN_POINT ( 'NONE',  ( -18.00000000000000355, -19.99999999999999289, -20.00000000000000000 ) ) ;
#3461 = ADVANCED_FACE ( 'NONE', ( #4560 ), #12188, .T. ) ;
#3462 = EDGE_LOOP ( 'NONE', ( #1735, #1414, #15069, #8475, #5824, #17918 ) ) ;
#3463 = CIRCLE ( 'NONE', #13479, 20.00000000000000000 ) ;
#3464 = CARTESIAN_POINT ( 'NONE',  ( 6.518095160331718319, 2.933089652807546077, -5.080260301817233426 ) ) ;
#3465 = CIRCLE ( 'NONE', #4729, 2.649999999999988809 ) ;
#3466 = VECTOR ( 'NONE', #18217, 1000.000000000000000 ) ;
#3467 = CARTESIAN_POINT ( 'NONE',  ( 56.65037692655921120, 47.10051614449766078, 2.184720259617097593 ) ) ;
#3468 = CARTESIAN_POINT ( 'NONE',  ( 52.25172492374522903, 61.59948385550239891, -7.007379884777225953 ) ) ;
#3469 = AXIS2_PLACEMENT_3D ( 'NONE', #14213, #14315, #1000 ) ;
#3470 = DIRECTION ( 'NONE',  ( 0.000000000000000000, 0.000000000000000000, 1.000000000000000000 ) ) ;
#3471 = ORIENTED_EDGE ( 'NONE', *, *, #10471, .T. ) ;
#3472 = DIRECTION ( 'NONE',  ( 2.191393683118470056E-17, 7.538405132783724027E-17, 1.000000000000000000 ) ) ;
#3473 = CARTESIAN_POINT ( 'NONE',  ( 9.037824375505316254, -2.158539001597377105, -9.000000000000000000 ) ) ;
#3474 = CARTESIAN_POINT ( 'NONE',  ( 49.97728705011488870, 61.49948385550241170, -6.000000000000000888 ) ) ;
#3475 = DIRECTION ( 'NONE',  ( -0.000000000000000000, -0.000000000000000000, 1.000000000000000000 ) ) ;
#3476 = PLANE ( 'NONE',  #12019 ) ;
#3477 = CARTESIAN_POINT ( 'NONE',  ( 57.61547081786810764, 60.90051614449766504, -2.450534656007114176 ) ) ;
#3478 = CIRCLE ( 'NONE', #972, 1.000000000000000000 ) ;
#3479 = CARTESIAN_POINT ( 'NONE',  ( 51.97223112728249816, 60.60051614449765367, -5.992620115222793586 ) ) ;
#3480 = FACE_OUTER_BOUND ( 'NONE', #473, .T. ) ;
#3481 = AXIS2_PLACEMENT_3D ( 'NONE', #13077, #8268, #7092 ) ;
#3482 = LINE ( 'NONE', #7972, #7826 ) ;
#3483 = VECTOR ( 'NONE', #8357, 1000.000000000000000 ) ;
#3484 = ORIENTED_EDGE ( 'NONE', *, *, #7051, .F. ) ;
#3485 = VERTEX_POINT ( 'NONE', #5933 ) ;
#3486 = FACE_OUTER_BOUND ( 'NONE', #4110, .T. ) ;
#3487 = ORIENTED_EDGE ( 'NONE', *, *, #591, .F. ) ;
#3488 = DIRECTION ( 'NONE',  ( 1.387778780781445676E-16, -1.000000000000000000, 0.000000000000000000 ) ) ;
#3489 = ORIENTED_EDGE ( 'NONE', *, *, #1242, .F. ) ;
#3490 = LINE ( 'NONE', #14052, #9084 ) ;
#3491 = CARTESIAN_POINT ( 'NONE',  ( 47.70284917648453415, 49.39948385550239607, -6.992620115222774047 ) ) ;
#3492 = VERTEX_POINT ( 'NONE', #18199 ) ;
#3493 = CARTESIAN_POINT ( 'NONE',  ( -0.1085714285714285687, -3.798448662927795372, -0.8000000000000000444 ) ) ;
#3494 = VECTOR ( 'NONE', #257, 999.9999999999998863 ) ;
#3495 = VERTEX_POINT ( 'NONE', #13568 ) ;
#3496 = CARTESIAN_POINT ( 'NONE',  ( 42.38452918213188525, 53.09948385550240602, -2.450534656007040013 ) ) ;
#3497 = AXIS2_PLACEMENT_3D ( 'NONE', #2075, #14115, #9598 ) ;
#3498 = CARTESIAN_POINT ( 'NONE',  ( 3.972073812946708582, -0.6951863858492246528, -3.565770933504603057 ) ) ;
#3499 = CARTESIAN_POINT ( 'NONE',  ( 42.63976443033212860, 64.99948385550240459, 0.02388180880522514787 ) ) ;
#3500 = CARTESIAN_POINT ( 'NONE',  ( 4.124214193018076458, 2.028338413290941222, -3.513185186763556622 ) ) ;
#3501 = AXIS2_PLACEMENT_3D ( 'NONE', #8941, #15121, #7664 ) ;
#3502 = DIRECTION ( 'NONE',  ( -0.000000000000000000, -0.000000000000000000, 1.000000000000000000 ) ) ;
#3503 = CARTESIAN_POINT ( 'NONE',  ( 43.33558569842706021, 63.90051614449765793, 2.141517661632167169 ) ) ;
#3504 = CARTESIAN_POINT ( 'NONE',  ( 6.367873360227558344, -2.886751345948133984, -5.000000000000000000 ) ) ;
#3505 = CARTESIAN_POINT ( 'NONE',  ( 43.34962307344081012, 60.89948385550241028, 2.184720259617164650 ) ) ;
#3506 = CARTESIAN_POINT ( 'NONE',  ( 75.00000000000000000, 32.50000000000001421, 15.00000000000000000 ) ) ;
#3507 = VERTEX_POINT ( 'NONE', #15228 ) ;
#3508 = ORIENTED_EDGE ( 'NONE', *, *, #7718, .F. ) ;
#3509 = DIRECTION ( 'NONE',  ( 0.000000000000000000, 0.000000000000000000, -1.000000000000000000 ) ) ;
#3510 = CARTESIAN_POINT ( 'NONE',  ( 44.03140696652192787, 51.19948385550238612, -4.306917132069425058 ) ) ;
#3511 = CIRCLE ( 'NONE', #13533, 5.000000000000000888 ) ;
#3512 = CARTESIAN_POINT ( 'NONE',  ( 4.200000000000001954, 2.449293598294707893E-16, -2.000000000000000888 ) ) ;
#3513 = VERTEX_POINT ( 'NONE', #11893 ) ;
#3514 = DIRECTION ( 'NONE',  ( -0.8090169943749487835, 0.5877852522924713607, 0.000000000000000000 ) ) ;
#3515 = ORIENTED_EDGE ( 'NONE', *, *, #14193, .F. ) ;
#3516 = DIRECTION ( 'NONE',  ( -0.000000000000000000, 0.000000000000000000, -1.000000000000000000 ) ) ;
#3517 = ORIENTED_EDGE ( 'NONE', *, *, #9516, .F. ) ;
#3518 = CARTESIAN_POINT ( 'NONE',  ( 47.74827507625478518, 46.59948385550239891, 7.007379884777227730 ) ) ;
#3519 = DIRECTION ( 'NONE',  ( -1.000000000000000000, -0.000000000000000000, -0.000000000000000000 ) ) ;
#3520 = CARTESIAN_POINT ( 'NONE',  ( 53.54508667620424234, 62.70051614449766220, -4.840751629271188961 ) ) ;
#3521 = PLANE ( 'NONE',  #3915 ) ;
#3522 = EDGE_CURVE ( 'NONE', #628, #7933, #140, .T. ) ;
#3523 = FACE_OUTER_BOUND ( 'NONE', #11989, .T. ) ;
#3524 = DIRECTION ( 'NONE',  ( 0.000000000000000000, 0.000000000000000000, 1.000000000000000000 ) ) ;
#3525 = CARTESIAN_POINT ( 'NONE',  ( 56.81924384183006538, 60.80051614449766362, -4.924951120819380357 ) ) ;
#3526 = EDGE_CURVE ( 'NONE', #5579, #13512, #3568, .T. ) ;
#3527 = ORIENTED_EDGE ( 'NONE', *, *, #2217, .F. ) ;
#3528 = ORIENTED_EDGE ( 'NONE', *, *, #7944, .F. ) ;
#3529 = CARTESIAN_POINT ( 'NONE',  ( -4.997494388800372001E-16, -0.4883827417527024095, 4.999999999999999112 ) ) ;
#3530 = SURFACE_STYLE_USAGE ( .BOTH. , #8313 ) ;
#3531 = EDGE_CURVE ( 'NONE', #9852, #1879, #615, .T. ) ;
#3532 = ADVANCED_FACE ( 'NONE', ( #12288 ), #6488, .T. ) ;
#3533 = DIRECTION ( 'NONE',  ( 1.000000000000000000, 0.000000000000000000, 0.000000000000000000 ) ) ;
#3534 = APPLICATION_PROTOCOL_DEFINITION ( 'draft international standard', 'automotive_design', 1998, #8651 ) ;
#3535 = VERTEX_POINT ( 'NONE', #3473 ) ;
#3536 = FACE_OUTER_BOUND ( 'NONE', #10820, .T. ) ;
#3537 = EDGE_CURVE ( 'NONE', #9381, #9166, #15718, .T. ) ;
#3538 = LINE ( 'NONE', #6663, #16611 ) ;
#3539 = ORIENTED_EDGE ( 'NONE', *, *, #10524, .F. ) ;
#3540 = CARTESIAN_POINT ( 'NONE',  ( 47.37792948025162332, 65.39948385550239607, -7.992620115222770494 ) ) ;
#3541 = DIRECTION ( 'NONE',  ( -1.000000000000000000, 0.000000000000000000, 0.000000000000000000 ) ) ;
#3542 = LINE ( 'NONE', #9314, #9848 ) ;
#3543 = DIRECTION ( 'NONE',  ( 0.000000000000000000, 0.000000000000000000, 1.000000000000000000 ) ) ;
#3544 = EDGE_CURVE ( 'NONE', #6895, #16099, #13754, .T. ) ;
#3545 = DIRECTION ( 'NONE',  ( 0.6691306063588675634, -0.7431448254773859174, 0.000000000000000000 ) ) ;
#3546 = EDGE_CURVE ( 'NONE', #10132, #10468, #3583, .T. ) ;
#3547 = CARTESIAN_POINT ( 'NONE',  ( 57.36023556966787851, 61.99948385550241170, -0.02388180880522424582 ) ) ;
#3548 = FACE_OUTER_BOUND ( 'NONE', #13996, .T. ) ;
#3549 = CARTESIAN_POINT ( 'NONE',  ( 42.38452918213188525, 57.09948385550240602, -2.450534656007040013 ) ) ;
#3550 = CARTESIAN_POINT ( 'NONE',  ( 55.94051828345053679, 61.20051614449766220, 4.345558710429044069 ) ) ;
#3551 = DIRECTION ( 'NONE',  ( -0.000000000000000000, -0.000000000000000000, 1.000000000000000000 ) ) ;
#3552 = DIRECTION ( 'NONE',  ( 0.9781476007338083534, -0.2079116908177467693, 0.000000000000000000 ) ) ;
#3553 = VERTEX_POINT ( 'NONE', #2298 ) ;
#3554 = CARTESIAN_POINT ( 'NONE',  ( 62.50000000000000000, 32.50000000000001421, 15.00000000000000000 ) ) ;
#3555 = CARTESIAN_POINT ( 'NONE',  ( 56.13503143586221000, 44.82443585060838132, -3.788959942617806220 ) ) ;
#3556 = CARTESIAN_POINT ( 'NONE',  ( 4.165266963751724560, -2.049631966911991565, 3.550066703508907739 ) ) ;
#3557 = FACE_OUTER_BOUND ( 'NONE', #18685, .T. ) ;
#3558 = VERTEX_POINT ( 'NONE', #18583 ) ;
#3559 = CARTESIAN_POINT ( 'NONE',  ( 0.9996874511566102850, -0.02500000000000036915, -9.000000000000000000 ) ) ;
#3560 = CARTESIAN_POINT ( 'NONE',  ( -20.63749999999999929, 0.000000000000000000, 0.000000000000000000 ) ) ;
#3561 = CARTESIAN_POINT ( 'NONE',  ( 49.97728705011488870, 63.49948385550241170, -6.000000000000000888 ) ) ;
#3562 = DIRECTION ( 'NONE',  ( 1.000000000000000000, 0.000000000000000000, 0.000000000000000000 ) ) ;
#3563 = DIRECTION ( 'NONE',  ( -1.000000000000000000, 0.000000000000000000, 0.000000000000000000 ) ) ;
#3564 = EDGE_CURVE ( 'NONE', #7908, #15389, #18289, .T. ) ;
#3565 = CARTESIAN_POINT ( 'NONE',  ( 62.49999999999998579, 45.00000000000001421, 15.00000000000000000 ) ) ;
#3566 = CARTESIAN_POINT ( 'NONE',  ( 57.61547081786810764, 62.90051614449765083, -2.450534656007114176 ) ) ;
#3567 = CARTESIAN_POINT ( 'NONE',  ( 51.92680522751238925, 63.40051614449765083, 6.007379884777208190 ) ) ;
#3568 = CIRCLE ( 'NONE', #17674, 3.799999999999999378 ) ;
#3569 = ADVANCED_FACE ( 'NONE', ( #9335 ), #4842, .T. ) ;
#3570 = CARTESIAN_POINT ( 'NONE',  ( -4.203833317240879275, -1.627343821129593859, -3.597273115243890818 ) ) ;
#3571 = DIRECTION ( 'NONE',  ( 0.000000000000000000, 0.000000000000000000, -1.000000000000000000 ) ) ;
#3572 = AXIS2_PLACEMENT_3D ( 'NONE', #19071, #15818, #5613 ) ;
#3573 = VERTEX_POINT ( 'NONE', #17007 ) ;
#3574 = VERTEX_POINT ( 'NONE', #10803 ) ;
#3575 = CARTESIAN_POINT ( 'NONE',  ( 3.098410542199072637, -7.060458129626440815, 0.000000000000000000 ) ) ;
#3576 = EDGE_LOOP ( 'NONE', ( #16872, #19115, #18912, #10241 ) ) ;
#3577 = B_SPLINE_CURVE_WITH_KNOTS ( 'NONE', 3,
 ( #83, #15166, #1941, #15255, #9361, #9082 ),
 .UNSPECIFIED., .F., .F.,
 ( 4, 2, 4 ),
 ( 0.003358874760055551890, 0.004541967308452098118, 0.005725059856848645212 ),
 .UNSPECIFIED. ) ;
#3578 = DIRECTION ( 'NONE',  ( 0.000000000000000000, -0.000000000000000000, 1.000000000000000000 ) ) ;
#3579 = ORIENTED_EDGE ( 'NONE', *, *, #883, .T. ) ;
#3580 = CARTESIAN_POINT ( 'NONE',  ( 0.1481481481481481122, -4.797713218419819903, 0.000000000000000000 ) ) ;
#3581 = CARTESIAN_POINT ( 'NONE',  ( 45.90387839640214196, 50.69948385550240744, 5.676469297603166098 ) ) ;
#3582 = EDGE_CURVE ( 'NONE', #15125, #273, #11092, .T. ) ;
#3583 = CIRCLE ( 'NONE', #15471, 1.535500000000000087 ) ;
#3584 = ORIENTED_EDGE ( 'NONE', *, *, #14917, .F. ) ;
#3585 = CARTESIAN_POINT ( 'NONE',  ( 6.506987859255520590, -2.925375531177299759, -5.066899051217866656 ) ) ;
#3586 = ORIENTED_EDGE ( 'NONE', *, *, #4960, .F. ) ;
#3587 = CARTESIAN_POINT ( 'NONE',  ( 41.58830220609386430, 50.99948385550241170, 0.02388180880523263147 ) ) ;
#3588 = AXIS2_PLACEMENT_3D ( 'NONE', #2781, #4732, #1399 ) ;
#3589 = LINE ( 'NONE', #8185, #9203 ) ;
#3590 = ADVANCED_FACE ( 'NONE', ( #3371 ), #447, .T. ) ;
#3591 = CARTESIAN_POINT ( 'NONE',  ( 47.74827507625478518, 64.59948385550239891, 7.007379884777227730 ) ) ;
#3592 = CARTESIAN_POINT ( 'NONE',  ( -159.0000000000000000, -14.99999999999999645, 17.00000000000000000 ) ) ;
#3593 = CARTESIAN_POINT ( 'NONE',  ( 4.175572532730933872, -4.122058607836120103, 1.048217341165752127E-14 ) ) ;
#3594 = CARTESIAN_POINT ( 'NONE',  ( 47.74827507625469281, 58.40051614449766504, -7.007379884777203749 ) ) ;
#3595 = CARTESIAN_POINT ( 'NONE',  ( 45.86712807150323812, 59.29948385550240175, -5.649768623646098220 ) ) ;
#3596 = CARTESIAN_POINT ( 'NONE',  ( 0.000000000000000000, 0.000000000000000000, 3.469446951953614189E-15 ) ) ;
#3597 = CARTESIAN_POINT ( 'NONE',  ( 53.50000000000000000, 0.000000000000000000, 0.000000000000000000 ) ) ;
#3598 = VERTEX_POINT ( 'NONE', #15328 ) ;
#3599 = EDGE_LOOP ( 'NONE', ( #8081, #7821, #19142, #10554 ) ) ;
#3600 = AXIS2_PLACEMENT_3D ( 'NONE', #18051, #1285, #7546 ) ;
#3601 = CARTESIAN_POINT ( 'NONE',  ( 45.90387839640214196, 52.69948385550240033, 5.676469297603166098 ) ) ;
#3602 = CARTESIAN_POINT ( 'NONE',  ( 9.999999999999994671, 20.00000000000001421, 15.00000000000000000 ) ) ;
#3603 = ORIENTED_EDGE ( 'NONE', *, *, #15982, .T. ) ;
#3604 = ORIENTED_EDGE ( 'NONE', *, *, #7528, .F. ) ;
#3605 = CARTESIAN_POINT ( 'NONE',  ( 0.3126073911696451990, -4.041451884327386779, -1.834154111220703958E-17 ) ) ;
#3606 = CIRCLE ( 'NONE', #13624, 0.4999999999999978351 ) ;
#3607 = ORIENTED_EDGE ( 'NONE', *, *, #10362, .F. ) ;
#3608 = CARTESIAN_POINT ( 'NONE',  ( 52.25172492374528588, 63.40051614449765083, 7.007379884777204637 ) ) ;
#3609 = VERTEX_POINT ( 'NONE', #15517 ) ;
#3610 = CARTESIAN_POINT ( 'NONE',  ( 55.94051828345050836, 45.79948385550240886, -4.345558710429104465 ) ) ;
#3611 = DIRECTION ( 'NONE',  ( 0.000000000000000000, 0.000000000000000000, -1.000000000000000000 ) ) ;
#3612 = CARTESIAN_POINT ( 'NONE',  ( 44.28664221472221385, 61.90051614449766504, 1.832500667257213722 ) ) ;
#3613 = LINE ( 'NONE', #7829, #15804 ) ;
#3614 = CARTESIAN_POINT ( 'NONE',  ( 6.445127866599365873, 3.194847394660948581, -4.687657648742338701 ) ) ;
#3615 = AXIS2_PLACEMENT_3D ( 'NONE', #2875, #11470, #2488 ) ;
#3616 = CARTESIAN_POINT ( 'NONE',  ( 45.31609314410960820, 58.30051614449765651, -6.485486291978072693 ) ) ;
#3617 = ORIENTED_EDGE ( 'NONE', *, *, #5063, .F. ) ;
#3618 = ORIENTED_EDGE ( 'NONE', *, *, #11802, .F. ) ;
#3619 = DIRECTION ( 'NONE',  ( -1.000000000000000000, 0.000000000000000000, 0.000000000000000000 ) ) ;
#3620 = FILL_AREA_STYLE_COLOUR ( '', #12154 ) ;
#3621 = B_SPLINE_CURVE_WITH_KNOTS ( 'NONE', 3,
 ( #18128, #17014, #10905, #16913 ),
 .UNSPECIFIED., .F., .F.,
 ( 4, 4 ),
 ( 0.000000000000000000, 0.002080789711329296236 ),
 .UNSPECIFIED. ) ;
#3622 = MECHANICAL_DESIGN_GEOMETRIC_PRESENTATION_REPRESENTATION (  '', ( #6750 ), #808 ) ;
#3623 = LINE ( 'NONE', #6557, #15017 ) ;
#3624 = CONTEXT_DEPENDENT_SHAPE_REPRESENTATION ( #14021, #16040 ) ;
#3625 = ORIENTED_EDGE ( 'NONE', *, *, #2815, .T. ) ;
#3626 = LINE ( 'NONE', #7934, #10493 ) ;
#3627 = ADVANCED_FACE ( 'NONE', ( #9527 ), #430, .T. ) ;
#3628 = CARTESIAN_POINT ( 'NONE',  ( 2.449293598294706513E-15, -20.00000000000000000, 15.00000000000000355 ) ) ;
#3629 = ORIENTED_EDGE ( 'NONE', *, *, #13705, .F. ) ;
#3630 = AXIS2_PLACEMENT_3D ( 'NONE', #4887, #11043, #6352 ) ;
#3631 = DIRECTION ( 'NONE',  ( 1.000000000000000000, 0.000000000000000000, 0.000000000000000000 ) ) ;
#3632 = DIRECTION ( 'NONE',  ( 0.000000000000000000, 0.000000000000000000, 1.000000000000000000 ) ) ;
#3633 = LINE ( 'NONE', #9594, #16433 ) ;
#3634 = EDGE_CURVE ( 'NONE', #1433, #2791, #19259, .T. ) ;
#3635 = EDGE_CURVE ( 'NONE', #6110, #444, #10769, .T. ) ;
#3636 = CARTESIAN_POINT ( 'NONE',  ( -0.6920835326022555245, -4.454600218803899558, -3.597382984111586079 ) ) ;
#3637 = AXIS2_PLACEMENT_3D ( 'NONE', #5992, #7548, #17859 ) ;
#3638 = CARTESIAN_POINT ( 'NONE',  ( 55.94051828345050836, 61.79948385550239465, -4.345558710429104465 ) ) ;
#3639 = DIRECTION ( 'NONE',  ( 0.000000000000000000, 0.000000000000000000, 1.000000000000000000 ) ) ;
#3640 = CARTESIAN_POINT ( 'NONE',  ( 42.38452918213188525, 61.09948385550241312, -2.450534656007040013 ) ) ;
#3641 = CARTESIAN_POINT ( 'NONE',  ( 56.66441430157294690, 60.90051614449766504, -2.141517661632166281 ) ) ;
#3642 = EDGE_CURVE ( 'NONE', #16030, #3706, #13935, .T. ) ;
#3643 = EDGE_CURVE ( 'NONE', #8396, #5344, #717, .T. ) ;
#3644 = DIRECTION ( 'NONE',  ( -0.000000000000000000, -0.000000000000000000, 1.000000000000000000 ) ) ;
#3645 = CARTESIAN_POINT ( 'NONE',  ( 1.000000000000000000, -14.00000000000000000, 8.999999999999998224 ) ) ;
#3646 = ORIENTED_EDGE ( 'NONE', *, *, #19396, .F. ) ;
#3647 = CARTESIAN_POINT ( 'NONE',  ( 2.449293598294706513E-15, -20.00000000000000000, -50.00000000000000000 ) ) ;
#3648 = EDGE_CURVE ( 'NONE', #10516, #8542, #18674, .T. ) ;
#3649 = PRODUCT ( 'spring', 'spring', '', ( #3253 ) ) ;
#3650 = EDGE_CURVE ( 'NONE', #11034, #2611, #3754, .T. ) ;
#3651 = LINE ( 'NONE', #9611, #3450 ) ;
#3652 = LINE ( 'NONE', #3366, #18836 ) ;
#3653 = CARTESIAN_POINT ( 'NONE',  ( 4.175813232069146785, -2.061359961916366057, 3.570380186727398542 ) ) ;
#3654 = DIRECTION ( 'NONE',  ( 0.000000000000000000, 0.000000000000000000, 1.000000000000000000 ) ) ;
#3655 = ORIENTED_EDGE ( 'NONE', *, *, #10145, .F. ) ;
#3656 = FACE_OUTER_BOUND ( 'NONE', #1540, .T. ) ;
#3657 = VECTOR ( 'NONE', #11746, 1000.000000000000000 ) ;
#3658 = DIRECTION ( 'NONE',  ( 0.000000000000000000, 0.000000000000000000, -1.000000000000000000 ) ) ;
#3659 = ADVANCED_FACE ( 'NONE', ( #16110, #18872, #1015 ), #10200, .F. ) ;
#3660 = CARTESIAN_POINT ( 'NONE',  ( -154.9999999999999716, -14.99999999999999645, 15.00000000000000000 ) ) ;
#3661 = DIRECTION ( 'NONE',  ( 0.000000000000000000, -1.224646799147353947E-16, 1.000000000000000000 ) ) ;
#3662 = CARTESIAN_POINT ( 'NONE',  ( -4.000000000000000000, 2.309401076758498483, -0.4999999999999927280 ) ) ;
#3663 = CARTESIAN_POINT ( 'NONE',  ( 52.62207051974829852, 62.60051614449765367, -7.992620115222797139 ) ) ;
#3664 = CARTESIAN_POINT ( 'NONE',  ( 51.97223112728249816, 62.60051614449765367, -5.992620115222793586 ) ) ;
#3665 = CLOSED_SHELL ( 'NONE', ( #12744, #3985, #12853, #8349, #18516, #5438, #292, #3767, #6678, #17555, #6889, #13970, #12563, #16730, #9982, #14712, #10503, #14422, #8605, #4240, #15488, #16842, #4392, #7709, #2701, #15768, #3049, #652, #7343 ) ) ;
#3666 = LINE ( 'NONE', #12679, #14427 ) ;
#3667 = CARTESIAN_POINT ( 'NONE',  ( -62.49999999999997158, 32.50000000000001421, -10.00000000000000178 ) ) ;
#3668 = ORIENTED_EDGE ( 'NONE', *, *, #6393, .T. ) ;
#3669 = ORIENTED_EDGE ( 'NONE', *, *, #16761, .T. ) ;
#3670 = DIRECTION ( 'NONE',  ( -0.000000000000000000, 0.000000000000000000, 1.000000000000000000 ) ) ;
#3671 = AXIS2_PLACEMENT_3D ( 'NONE', #18629, #2258, #12918 ) ;
#3672 = ORIENTED_EDGE ( 'NONE', *, *, #13945, .T. ) ;
#3673 = CARTESIAN_POINT ( 'NONE',  ( -62.49999999999997158, 32.50000000000001421, 15.00000000000000000 ) ) ;
#3674 = ORIENTED_EDGE ( 'NONE', *, *, #2461, .T. ) ;
#3675 = DIRECTION ( 'NONE',  ( -0.000000000000000000, -0.000000000000000000, 1.000000000000000000 ) ) ;
#3676 = CARTESIAN_POINT ( 'NONE',  ( 52.29715082351547295, 58.39948385550240317, 6.992620115222774047 ) ) ;
#3677 = ORIENTED_EDGE ( 'NONE', *, *, #11589, .F. ) ;
#3678 = DIRECTION ( 'NONE',  ( -0.000000000000000000, -0.000000000000000000, 1.000000000000000000 ) ) ;
#3679 = EDGE_LOOP ( 'NONE', ( #13028, #5445, #10377, #12934 ) ) ;
#3680 = AXIS2_PLACEMENT_3D ( 'NONE', #1496, #7469, #17980 ) ;
#3681 = CARTESIAN_POINT ( 'NONE',  ( 56.81924384183011512, 50.19948385550241454, 4.924951120819313743 ) ) ;
#3682 = FACE_OUTER_BOUND ( 'NONE', #14626, .T. ) ;
#3683 = CIRCLE ( 'NONE', #11491, 1.000000000000000444 ) ;
#3684 = CARTESIAN_POINT ( 'NONE',  ( 45.90387839640214196, 62.69948385550240744, 5.676469297603166098 ) ) ;
#3685 = CARTESIAN_POINT ( 'NONE',  ( 3.880206590543030742, 2.665671387532550618, 2.382921720510995822 ) ) ;
#3686 = CARTESIAN_POINT ( 'NONE',  ( -154.8505191518487152, -18.79705879280739467, -15.79999999999999893 ) ) ;
#3687 = VECTOR ( 'NONE', #3502, 1000.000000000000000 ) ;
#3688 = CARTESIAN_POINT ( 'NONE',  ( 47.70284917648459100, 57.60051614449764656, 6.992620115222796251 ) ) ;
#3689 = CARTESIAN_POINT ( 'NONE',  ( 51.97223112728254790, 62.39948385550240317, 5.992620115222778487 ) ) ;
#3690 = CARTESIAN_POINT ( 'NONE',  ( 57.36023556966787851, 57.99948385550239038, -0.02388180880522424582 ) ) ;
#3691 = CARTESIAN_POINT ( 'NONE',  ( 6.420058897733096792, -2.891482565094587898, 5.008194711943423805 ) ) ;
#3692 = CARTESIAN_POINT ( 'NONE',  ( -4.000000000000000000, -0.3979232138631226823, -3.896351557369779711E-17 ) ) ;
#3693 = ORIENTED_EDGE ( 'NONE', *, *, #9073, .F. ) ;
#3694 = ADVANCED_FACE ( 'NONE', ( #5714 ), #2690, .F. ) ;
#3695 = AXIS2_PLACEMENT_3D ( 'NONE', #1204, #8554, #5318 ) ;
#3696 = VERTEX_POINT ( 'NONE', #1105 ) ;
#3697 = FACE_OUTER_BOUND ( 'NONE', #12688, .T. ) ;
#3698 = SURFACE_SIDE_STYLE ('',( #12515 ) ) ;
#3699 = EDGE_CURVE ( 'NONE', #12768, #12590, #15294, .T. ) ;
#3700 = AXIS2_PLACEMENT_3D ( 'NONE', #12562, #3644, #18372 ) ;
#3701 = CARTESIAN_POINT ( 'NONE',  ( 52.29715082351547295, 54.39948385550239607, 6.992620115222774047 ) ) ;
#3702 = DIRECTION ( 'NONE',  ( 0.000000000000000000, -0.000000000000000000, 1.000000000000000000 ) ) ;
#3703 = VERTEX_POINT ( 'NONE', #11290 ) ;
#3704 = VERTEX_POINT ( 'NONE', #14327 ) ;
#3705 = CARTESIAN_POINT ( 'NONE',  ( 62.49999999999998579, 20.00000000000001421, 15.00000000000000000 ) ) ;
#3706 = VERTEX_POINT ( 'NONE', #8252 ) ;
#3707 = CARTESIAN_POINT ( 'NONE',  ( 57.36023556966787851, 63.00051614449767357, 0.02388180880515038476 ) ) ;
#3708 = VERTEX_POINT ( 'NONE', #12869 ) ;
#3709 = FACE_OUTER_BOUND ( 'NONE', #3462, .T. ) ;
#3710 = LINE ( 'NONE', #18922, #7728 ) ;
#3711 = CARTESIAN_POINT ( 'NONE',  ( 43.69122665457040000, 60.00051614449765935, -0.02388180880515696977 ) ) ;
#3712 = CARTESIAN_POINT ( 'NONE',  ( 2.449293598294706513E-15, -20.00000000000000000, 15.00000000000000355 ) ) ;
#3713 = CIRCLE ( 'NONE', #7462, 20.00000000000000000 ) ;
#3714 = AXIS2_PLACEMENT_3D ( 'NONE', #14584, #5179, #776 ) ;
#3715 = DIRECTION ( 'NONE',  ( -1.224646799147353207E-16, 0.000000000000000000, -1.000000000000000000 ) ) ;
#3716 = FACE_BOUND ( 'NONE', #13521, .T. ) ;
#3717 = CARTESIAN_POINT ( 'NONE',  ( 43.18075615816994173, 61.80051614449766362, 4.924951120819380357 ) ) ;
#3718 = ORIENTED_EDGE ( 'NONE', *, *, #17333, .F. ) ;
#3719 = VERTEX_POINT ( 'NONE', #8643 ) ;
#3720 = DIRECTION ( 'NONE',  ( 0.000000000000000000, -0.000000000000000000, 1.000000000000000000 ) ) ;
#3721 = PRESENTATION_STYLE_ASSIGNMENT (( #13820 ) ) ;
#3722 = EDGE_LOOP ( 'NONE', ( #19194, #9901 ) ) ;
#3723 = CARTESIAN_POINT ( 'NONE',  ( -154.9999999999999716, -14.99999999999999645, 15.00000000000000000 ) ) ;
#3724 = VECTOR ( 'NONE', #17343, 1000.000000000000000 ) ;
#3725 = AXIS2_PLACEMENT_3D ( 'NONE', #13000, #5542, #12708 ) ;
#3726 = LINE ( 'NONE', #10975, #959 ) ;
#3727 = VERTEX_POINT ( 'NONE', #5410 ) ;
#3728 = DIRECTION ( 'NONE',  ( 0.9781476007338083534, -0.2079116908177467693, 0.000000000000000000 ) ) ;
#3729 = CARTESIAN_POINT ( 'NONE',  ( 4.799999999999999822, 0.000000000000000000, -1.000000000000000000 ) ) ;
#3730 = MECHANICAL_DESIGN_GEOMETRIC_PRESENTATION_REPRESENTATION (  '', ( #14055 ), #11233 ) ;
#3731 = CARTESIAN_POINT ( 'NONE',  ( 0.000000000000000000, 0.000000000000000000, 10.00000000000000000 ) ) ;
#3732 = DIRECTION ( 'NONE',  ( 0.000000000000000000, -0.000000000000000000, 1.000000000000000000 ) ) ;
#3733 = CARTESIAN_POINT ( 'NONE',  ( 4.000000000000003553, 0.000000000000000000, 0.000000000000000000 ) ) ;
#3734 = CARTESIAN_POINT ( 'NONE',  ( 50.02271294988512551, 62.49948385550240459, 7.000000000000000888 ) ) ;
#3735 = CARTESIAN_POINT ( 'NONE',  ( 6.355827204229362870, 3.436818823786758070, 4.264647808192652434 ) ) ;
#3736 = CARTESIAN_POINT ( 'NONE',  ( 49.97728705011486738, 65.49948385550240459, -8.000000000000001776 ) ) ;
#3737 = VECTOR ( 'NONE', #14659, 1000.000000000000000 ) ;
#3738 = ADVANCED_FACE ( 'NONE', ( #17595 ), #2498, .T. ) ;
#3739 = CARTESIAN_POINT ( 'NONE',  ( 42.63976443033212860, 64.00051614449765225, -0.02388180880514948964 ) ) ;
#3740 = AXIS2_PLACEMENT_3D ( 'NONE', #11015, #2213, #17022 ) ;
#3741 = LINE ( 'NONE', #18275, #14641 ) ;
#3742 = DIRECTION ( 'NONE',  ( 1.000000000000000000, 0.000000000000000000, 0.000000000000000000 ) ) ;
#3743 = AXIS2_PLACEMENT_3D ( 'NONE', #16107, #13342, #10402 ) ;
#3744 = ORIENTED_EDGE ( 'NONE', *, *, #6811, .F. ) ;
#3745 = DIRECTION ( 'NONE',  ( 0.000000000000000000, -0.5000000000000001110, 0.8660254037844387076 ) ) ;
#3746 = CARTESIAN_POINT ( 'NONE',  ( 0.1999999999999985678, -6.997142273814360713, -0.8000000000000000444 ) ) ;
#3747 = CARTESIAN_POINT ( 'NONE',  ( 47.74827507625470702, 50.40051614449765793, -7.007379884777204637 ) ) ;
#3748 = CIRCLE ( 'NONE', #14701, 8.000000000000000000 ) ;
#3749 = CARTESIAN_POINT ( 'NONE',  ( 53.94396537754659704, 44.99999999999997158, -6.362703256440709332 ) ) ;
#3750 = EDGE_CURVE ( 'NONE', #976, #4855, #11582, .T. ) ;
#3751 = PLANE ( 'NONE',  #16530 ) ;
#3752 = VERTEX_POINT ( 'NONE', #910 ) ;
#3753 = DIRECTION ( 'NONE',  ( 0.000000000000000000, 0.000000000000000000, 1.000000000000000000 ) ) ;
#3754 = LINE ( 'NONE', #9913, #1081 ) ;
#3755 = CARTESIAN_POINT ( 'NONE',  ( 0.1999999999999985678, -6.997142273814360713, 0.000000000000000000 ) ) ;
#3756 = CARTESIAN_POINT ( 'NONE',  ( 45.86712807150323812, 47.29948385550240886, -5.649768623646098220 ) ) ;
#3757 = DIRECTION ( 'NONE',  ( 0.4999999999999974465, 0.8660254037844401509, 0.000000000000000000 ) ) ;
#3758 = CARTESIAN_POINT ( 'NONE',  ( 56.81924384183006538, 58.80051614449766362, -4.924951120819380357 ) ) ;
#3759 = EDGE_CURVE ( 'NONE', #8619, #9062, #16203, .T. ) ;
#3760 = CARTESIAN_POINT ( 'NONE',  ( 55.11794222512599362, 62.80051614449766362, -3.688883143319583446 ) ) ;
#3761 = EDGE_CURVE ( 'NONE', #17070, #7670, #11391, .T. ) ;
#3762 = EDGE_CURVE ( 'NONE', #17113, #3828, #4149, .T. ) ;
#3763 = CARTESIAN_POINT ( 'NONE',  ( 1.925929944387235853E-31, 15.00000000000001599, 15.00000000000000000 ) ) ;
#3764 = CARTESIAN_POINT ( 'NONE',  ( 6.506891485183659896, -2.992470280394939675, 5.000000000000000000 ) ) ;
#3765 = AXIS2_PLACEMENT_3D ( 'NONE', #6190, #9408, #15301 ) ;
#3766 = EDGE_LOOP ( 'NONE', ( #6274, #11337, #16028, #14176, #7839 ) ) ;
#3767 = ADVANCED_FACE ( 'NONE', ( #16016 ), #18769, .F. ) ;
#3768 = ORIENTED_EDGE ( 'NONE', *, *, #15402, .T. ) ;
#3769 = AXIS2_PLACEMENT_3D ( 'NONE', #10862, #18440, #4987 ) ;
#3770 = AXIS2_PLACEMENT_3D ( 'NONE', #3013, #6233, #19412 ) ;
#3771 = VERTEX_POINT ( 'NONE', #19172 ) ;
#3772 = CARTESIAN_POINT ( 'NONE',  ( 2.449293598294706513E-15, -20.00000000000000000, -10.00000000000000000 ) ) ;
#3773 = EDGE_LOOP ( 'NONE', ( #4351, #18109, #16076, #18032 ) ) ;
#3774 = ADVANCED_FACE ( 'NONE', ( #17297 ), #9815, .T. ) ;
#3775 = CARTESIAN_POINT ( 'NONE',  ( -10.93224627749297362, -36.74771600333134813, -9.000000000000000000 ) ) ;
#3776 = AXIS2_PLACEMENT_3D ( 'NONE', #4245, #4545, #4452 ) ;
#3777 = ORIENTED_EDGE ( 'NONE', *, *, #18984, .T. ) ;
#3778 = CARTESIAN_POINT ( 'NONE',  ( 3.999999999999999112, 2.309401076758497595, -3.504271511726784194 ) ) ;
#3779 = CARTESIAN_POINT ( 'NONE',  ( 56.65037692655918988, 55.89948385550240317, -2.184720259617163762 ) ) ;
#3780 = ORIENTED_EDGE ( 'NONE', *, *, #16013, .T. ) ;
#3781 = CARTESIAN_POINT ( 'NONE',  ( 32.00000000000000000, -3.000000000000000000, 6.000000000000003553 ) ) ;
#3782 = ORIENTED_EDGE ( 'NONE', *, *, #16606, .T. ) ;
#3783 = CARTESIAN_POINT ( 'NONE',  ( 54.68390685589033495, 51.69948385550241454, -6.485486291978119766 ) ) ;
#3784 = CIRCLE ( 'NONE', #11592, 1.000000000000001110 ) ;
#3785 = DIRECTION ( 'NONE',  ( 1.000000000000000000, 0.000000000000000000, 0.000000000000000000 ) ) ;
#3786 = CARTESIAN_POINT ( 'NONE',  ( 45.86712807150323812, 65.29948385550241596, -5.649768623646098220 ) ) ;
#3787 = DIRECTION ( 'NONE',  ( 0.000000000000000000, 0.000000000000000000, 1.000000000000000000 ) ) ;
#3788 = CARTESIAN_POINT ( 'NONE',  ( 4.124214193018072017, -4.056676826581893103, 6.968404583626299416E-17 ) ) ;
#3789 = CIRCLE ( 'NONE', #10979, 4.000000000000003553 ) ;
#3790 = AXIS2_PLACEMENT_3D ( 'NONE', #11602, #3871, #14247 ) ;
#3791 = CARTESIAN_POINT ( 'NONE',  ( 49.97728705011495265, 61.50051614449765935, 7.000000000000000888 ) ) ;
#3792 = EDGE_CURVE ( 'NONE', #8294, #12345, #18966, .T. ) ;
#3793 = CARTESIAN_POINT ( 'NONE',  ( 51.92680522751233951, 61.59948385550240602, -6.007379884777223289 ) ) ;
#3794 = EDGE_CURVE ( 'NONE', #14540, #4021, #8453, .T. ) ;
#3795 = CARTESIAN_POINT ( 'NONE',  ( 54.09612160359786515, 59.69948385550240033, -5.676469297603166098 ) ) ;
#3796 = DIRECTION ( 'NONE',  ( -1.000000000000000000, 0.000000000000000000, 0.000000000000000000 ) ) ;
#3797 = CARTESIAN_POINT ( 'NONE',  ( 2.482347295856823136E-15, -20.00000000000000000, -8.999999999999996447 ) ) ;
#3798 = ORIENTED_EDGE ( 'NONE', *, *, #16836, .T. ) ;
#3799 = ORIENTED_EDGE ( 'NONE', *, *, #16660, .T. ) ;
#3800 = DIRECTION ( 'NONE',  ( -1.000000000000000000, 0.000000000000000000, -0.000000000000000000 ) ) ;
#3801 = ORIENTED_EDGE ( 'NONE', *, *, #6851, .F. ) ;
#3802 = CARTESIAN_POINT ( 'NONE',  ( 47.70284917648453415, 61.39948385550241738, -6.992620115222774047 ) ) ;
#3803 = PLANE ( 'NONE',  #16893 ) ;
#3804 = AXIS2_PLACEMENT_3D ( 'NONE', #16960, #2349, #858 ) ;
#3805 = ORIENTED_EDGE ( 'NONE', *, *, #14960, .T. ) ;
#3806 = CIRCLE ( 'NONE', #41, 1.535500000000000087 ) ;
#3807 = VERTEX_POINT ( 'NONE', #2600 ) ;
#3808 = CARTESIAN_POINT ( 'NONE',  ( -151.2002204621512078, -14.95906757097668027, -15.79999999999999893 ) ) ;
#3809 = ORIENTED_EDGE ( 'NONE', *, *, #525, .T. ) ;
#3810 = DIRECTION ( 'NONE',  ( -0.000000000000000000, -0.000000000000000000, -1.000000000000000000 ) ) ;
#3811 = VERTEX_POINT ( 'NONE', #11480 ) ;
#3812 = CARTESIAN_POINT ( 'NONE',  ( 0.000000000000000000, 4.330127018922190096, -2.500000000000006217 ) ) ;
#3813 = CARTESIAN_POINT ( 'NONE',  ( -154.9999999999999716, -6.999999999999993783, -15.00000000000000000 ) ) ;
#3814 = CARTESIAN_POINT ( 'NONE',  ( 50.02271294988505446, 44.50051614449765935, -7.000000000000000888 ) ) ;
#3815 = DIRECTION ( 'NONE',  ( 0.02857142857142857401, -0.9995917534020515305, 0.000000000000000000 ) ) ;
#3816 = ADVANCED_FACE ( 'NONE', ( #17489 ), #8552, .F. ) ;
#3817 = EDGE_CURVE ( 'NONE', #5258, #3064, #8966, .T. ) ;
#3818 = DIRECTION ( 'NONE',  ( 1.000000000000000000, 0.000000000000000000, 0.000000000000000000 ) ) ;
#3819 = AXIS2_PLACEMENT_3D ( 'NONE', #3053, #2864, #8 ) ;
#3820 = EDGE_CURVE ( 'NONE', #1464, #8101, #12968, .T. ) ;
#3821 = AXIS2_PLACEMENT_3D ( 'NONE', #19273, #5812, #7082 ) ;
#3822 = ORIENTED_EDGE ( 'NONE', *, *, #1758, .T. ) ;
#3823 = VERTEX_POINT ( 'NONE', #8843 ) ;
#3824 = CARTESIAN_POINT ( 'NONE',  ( 4.197478902586992966, -0.8524102783748346290, -3.505063281295504041 ) ) ;
#3825 =( NAMED_UNIT ( * ) PLANE_ANGLE_UNIT ( ) SI_UNIT ( $, .RADIAN. ) );
#3826 = DIRECTION ( 'NONE',  ( -0.000000000000000000, -0.000000000000000000, 1.000000000000000000 ) ) ;
#3827 = LINE ( 'NONE', #13126, #2151 ) ;
#3828 = VERTEX_POINT ( 'NONE', #17776 ) ;
#3829 = CARTESIAN_POINT ( 'NONE',  ( 2.482347295856823136E-15, -20.00000000000000000, -8.999999999999996447 ) ) ;
#3830 = DIRECTION ( 'NONE',  ( 0.000000000000000000, 0.000000000000000000, -1.000000000000000000 ) ) ;
#3831 = ORIENTED_EDGE ( 'NONE', *, *, #9143, .F. ) ;
#3832 = EDGE_CURVE ( 'NONE', #8753, #9638, #14850, .T. ) ;
#3833 = CARTESIAN_POINT ( 'NONE',  ( 0.000000000000000000, 0.000000000000000000, 0.000000000000000000 ) ) ;
#3834 = DIRECTION ( 'NONE',  ( -0.000000000000000000, -0.000000000000000000, 1.000000000000000000 ) ) ;
#3835 = FACE_OUTER_BOUND ( 'NONE', #14022, .T. ) ;
#3836 = EDGE_CURVE ( 'NONE', #14054, #3297, #3280, .T. ) ;
#3837 = FACE_OUTER_BOUND ( 'NONE', #760, .T. ) ;
#3838 = CARTESIAN_POINT ( 'NONE',  ( 55.11794222512601493, 48.19948385550240744, 3.688883143319541702 ) ) ;
#3839 = CARTESIAN_POINT ( 'NONE',  ( 3.951447005078450925, -2.357513599190977249, -2.916666666666666519 ) ) ;
#3840 = CARTESIAN_POINT ( 'NONE',  ( 44.03140696652192787, 49.19948385550240033, -4.306917132069425058 ) ) ;
#3841 = CARTESIAN_POINT ( 'NONE',  ( 47.70284917648459100, 59.60051614449765367, 6.992620115222796251 ) ) ;
#3842 = AXIS2_PLACEMENT_3D ( 'NONE', #6622, #12599, #5148 ) ;
#3843 = DIRECTION ( 'NONE',  ( 0.000000000000000000, -1.000000000000000000, 8.673617379884036458E-16 ) ) ;
#3844 = CARTESIAN_POINT ( 'NONE',  ( 6.323279575527231522, 3.325091652218045368, -4.240772318537636920 ) ) ;
#3845 = DIRECTION ( 'NONE',  ( 6.123233995736766036E-17, 0.000000000000000000, 1.000000000000000000 ) ) ;
#3846 = ORIENTED_EDGE ( 'NONE', *, *, #294, .T. ) ;
#3847 = LINE ( 'NONE', #12760, #5472 ) ;
#3848 = FACE_OUTER_BOUND ( 'NONE', #3950, .T. ) ;
#3849 = CARTESIAN_POINT ( 'NONE',  ( 54.09612160359792199, 55.30051614449765651, 5.676469297603124353 ) ) ;
#3850 = CARTESIAN_POINT ( 'NONE',  ( -99.99999999999997158, -23.00000000000000711, -10.00000000000000178 ) ) ;
#3851 = CARTESIAN_POINT ( 'NONE',  ( 55.32279841668061238, 44.85244137215321558, -4.999999999999997335 ) ) ;
#3852 = ORIENTED_EDGE ( 'NONE', *, *, #6062, .F. ) ;
#3853 = DIRECTION ( 'NONE',  ( -1.000000000000000000, -0.000000000000000000, -0.000000000000000000 ) ) ;
#3854 = CARTESIAN_POINT ( 'NONE',  ( 0.000000000000000000, 4.330127018922190985, 2.500000000000005329 ) ) ;
#3855 = DIRECTION ( 'NONE',  ( 1.000000000000000000, 0.000000000000000000, 0.000000000000000000 ) ) ;
#3856 = CARTESIAN_POINT ( 'NONE',  ( 43.34962307344081012, 46.89948385550240317, 2.184720259617164650 ) ) ;
#3857 = AXIS2_PLACEMENT_3D ( 'NONE', #5703, #7364, #4433 ) ;
#3858 = CYLINDRICAL_SURFACE ( 'NONE', #10140, 4.000000000000000000 ) ;
#3859 = CARTESIAN_POINT ( 'NONE',  ( 52.57664461997821093, 63.40051614449765083, 8.007379884777206414 ) ) ;
#3860 = CARTESIAN_POINT ( 'NONE',  ( -62.49999999999997158, 40.00000000000001421, -9.999999999999998224 ) ) ;
#3861 = CARTESIAN_POINT ( 'NONE',  ( 46.49166364869456913, 60.30051614449767072, -4.867452303228181343 ) ) ;
#3862 = DIRECTION ( 'NONE',  ( 0.4999999999999974465, 0.8660254037844401509, 0.000000000000000000 ) ) ;
#3863 = LINE ( 'NONE', #5224, #17563 ) ;
#3864 = EDGE_LOOP ( 'NONE', ( #6325, #14684, #12211, #4511 ) ) ;
#3865 = ORIENTED_EDGE ( 'NONE', *, *, #4848, .T. ) ;
#3866 = ORIENTED_EDGE ( 'NONE', *, *, #12259, .F. ) ;
#3867 = DIRECTION ( 'NONE',  ( 1.000000000000000000, 0.000000000000000000, 0.000000000000000000 ) ) ;
#3868 = ORIENTED_EDGE ( 'NONE', *, *, #9565, .F. ) ;
#3869 = FACE_OUTER_BOUND ( 'NONE', #4573, .T. ) ;
#3870 = ORIENTED_EDGE ( 'NONE', *, *, #1130, .T. ) ;
#3871 = DIRECTION ( 'NONE',  ( 0.000000000000000000, 0.000000000000000000, 1.000000000000000000 ) ) ;
#3872 = ADVANCED_FACE ( 'NONE', ( #14819 ), #14720, .T. ) ;
#3873 = CARTESIAN_POINT ( 'NONE',  ( 49.97728705011488159, 57.49948385550241170, -7.000000000000000888 ) ) ;
#3874 = B_SPLINE_CURVE_WITH_KNOTS ( 'NONE', 3,
 ( #6764, #6856, #12843, #3934, #14406, #2476 ),
 .UNSPECIFIED., .F., .F.,
 ( 4, 2, 4 ),
 ( 0.005852013098461904955, 0.006875955139453157790, 0.007899897180444410624 ),
 .UNSPECIFIED. ) ;
#3875 = ORIENTED_EDGE ( 'NONE', *, *, #13050, .F. ) ;
#3876 = LINE ( 'NONE', #11406, #16818 ) ;
#3877 = ORIENTED_EDGE ( 'NONE', *, *, #3642, .T. ) ;
#3878 = CARTESIAN_POINT ( 'NONE',  ( 54.72065718078924590, 54.29948385550241596, 6.458785618021043895 ) ) ;
#3879 = DIRECTION ( 'NONE',  ( 0.000000000000000000, 0.000000000000000000, 1.000000000000000000 ) ) ;
#3880 = ADVANCED_FACE ( 'NONE', ( #10496 ), #7375, .T. ) ;
#3881 = CARTESIAN_POINT ( 'NONE',  ( 55.08986747509847248, 47.79948385550240886, -3.727524721679197572 ) ) ;
#3882 = AXIS2_PLACEMENT_3D ( 'NONE', #2226, #6713, #13871 ) ;
#3883 = DIRECTION ( 'NONE',  ( 0.000000000000000000, 0.000000000000000000, 1.000000000000000000 ) ) ;
#3884 = DIRECTION ( 'NONE',  ( -1.000000000000000000, 0.000000000000000000, 0.000000000000000000 ) ) ;
#3885 = CARTESIAN_POINT ( 'NONE',  ( 56.79116909180259398, 45.20051614449766220, 4.963592699178938972 ) ) ;
#3886 = EDGE_CURVE ( 'NONE', #12017, #2369, #13345, .T. ) ;
#3887 = CARTESIAN_POINT ( 'NONE',  ( 44.91013252490152752, 62.79948385550240175, 3.727524721679198461 ) ) ;
#3888 = EDGE_CURVE ( 'NONE', #8758, #75, #13252, .T. ) ;
#3889 = CARTESIAN_POINT ( 'NONE',  ( -4.872650870659752442, 0.4273491293402474911, -0.8000000000000000444 ) ) ;
#3890 = DIRECTION ( 'NONE',  ( 1.000000000000000000, 0.000000000000000000, 0.000000000000000000 ) ) ;
#3891 = EDGE_LOOP ( 'NONE', ( #12395, #17263 ) ) ;
#3892 = ADVANCED_FACE ( 'NONE', ( #14919 ), #19367, .F. ) ;
#3893 = ORIENTED_EDGE ( 'NONE', *, *, #6521, .F. ) ;
#3894 = DIRECTION ( 'NONE',  ( 1.000000000000000000, 0.000000000000000000, 0.000000000000000000 ) ) ;
#3895 = SURFACE_SIDE_STYLE ('',( #5067 ) ) ;
#3896 = EDGE_LOOP ( 'NONE', ( #7677, #3272, #11341, #7131 ) ) ;
#3897 = CARTESIAN_POINT ( 'NONE',  ( 50.02271294988512551, 58.49948385550241170, 7.000000000000000888 ) ) ;
#3898 = CARTESIAN_POINT ( 'NONE',  ( 0.1085714285714285687, -3.798448662927795372, 0.000000000000000000 ) ) ;
#3899 = ORIENTED_EDGE ( 'NONE', *, *, #11297, .T. ) ;
#3900 = ORIENTED_EDGE ( 'NONE', *, *, #4144, .T. ) ;
#3901 = VECTOR ( 'NONE', #7855, 1000.000000000000000 ) ;
#3902 = DIRECTION ( 'NONE',  ( 1.000000000000000000, 0.000000000000000000, 0.000000000000000000 ) ) ;
#3903 = EDGE_CURVE ( 'NONE', #8366, #7648, #8936, .T. ) ;
#3904 = EDGE_CURVE ( 'NONE', #5077, #8618, #6388, .T. ) ;
#3905 = ORIENTED_EDGE ( 'NONE', *, *, #2081, .F. ) ;
#3906 = DIRECTION ( 'NONE',  ( 1.000000000000000000, 0.000000000000000000, 0.000000000000000000 ) ) ;
#3907 = EDGE_LOOP ( 'NONE', ( #12635, #19029, #3342, #11438 ) ) ;
#3908 = CARTESIAN_POINT ( 'NONE',  ( 55.96859303347804371, 52.19948385550240033, 4.306917132069425946 ) ) ;
#3909 = CYLINDRICAL_SURFACE ( 'NONE', #18400, 1.000000000000000888 ) ;
#3910 = CARTESIAN_POINT ( 'NONE',  ( 53.50833635130544508, 59.30051614449766362, 4.867452303228181343 ) ) ;
#3911 = CARTESIAN_POINT ( 'NONE',  ( 3.020236159542450949, -23.98474259401938014, 15.00000000000000355 ) ) ;
#3912 =( NAMED_UNIT ( * ) SI_UNIT ( $, .STERADIAN. ) SOLID_ANGLE_UNIT ( ) );
#3913 = B_SPLINE_CURVE_WITH_KNOTS ( 'NONE', 3,
 ( #18291, #6317, #6594, #9529, #4844, #15520 ),
 .UNSPECIFIED., .F., .F.,
 ( 4, 2, 4 ),
 ( 4.336808689942017736E-19, 0.0002095117440854729585, 0.0004190234881709454834 ),
 .UNSPECIFIED. ) ;
#3914 = LINE ( 'NONE', #8307, #7534 ) ;
#3915 = AXIS2_PLACEMENT_3D ( 'NONE', #2053, #8016, #573 ) ;
#3916 = VERTEX_POINT ( 'NONE', #3074 ) ;
#3917 = EDGE_LOOP ( 'NONE', ( #10067, #2333, #5423 ) ) ;
#3918 = CARTESIAN_POINT ( 'NONE',  ( 2.449293598294706513E-15, -20.00000000000000000, -9.000000000000000000 ) ) ;
#3919 =( NAMED_UNIT ( * ) SI_UNIT ( $, .STERADIAN. ) SOLID_ANGLE_UNIT ( ) );
#3920 =( GEOMETRIC_REPRESENTATION_CONTEXT ( 3 ) GLOBAL_UNCERTAINTY_ASSIGNED_CONTEXT ( ( #100 ) ) GLOBAL_UNIT_ASSIGNED_CONTEXT ( ( #14123, #2291, #17288 ) ) REPRESENTATION_CONTEXT ( 'NONE', 'WORKASPACE' ) );
#3921 = LINE ( 'NONE', #8614, #1185 ) ;
#3922 = CARTESIAN_POINT ( 'NONE',  ( 0.3126073911696408136, 2.020725942163688060, 3.500000000000000000 ) ) ;
#3923 = VERTEX_POINT ( 'NONE', #7566 ) ;
#3924 = CARTESIAN_POINT ( 'NONE',  ( 6.204460410672266946, 4.828986228461177532, 1.635950503255240607 ) ) ;
#3925 = AXIS2_PLACEMENT_3D ( 'NONE', #7852, #408, #8133 ) ;
#3926 = ORIENTED_EDGE ( 'NONE', *, *, #18352, .T. ) ;
#3927 =( BOUNDED_SURFACE ( )  B_SPLINE_SURFACE ( 3, 2, ( 
 ( #1697, #7380, #13553 ),
 ( #16506, #3079, #15023 ),
 ( #8849, #6106, #10701 ),
 ( #7474, #2976, #17984 ),
 ( #10308, #14824, #13454 ),
 ( #2889, #16604, #14925 ) ),
 .UNSPECIFIED., .F., .F., .T. ) 
 B_SPLINE_SURFACE_WITH_KNOTS ( ( 4, 2, 4 ),
 ( 3, 3 ),
 ( 0.01651999345535506980, 0.01858032176739836394, 0.02064065007944165808 ),
 ( 0.000000000000000000, 1.000000000000000000 ),
 .UNSPECIFIED. ) 
 GEOMETRIC_REPRESENTATION_ITEM ( )  RATIONAL_B_SPLINE_SURFACE ( (
 ( 1.000000000000000000, 0.8047781103519393575, 1.000000000000000000),
 ( 1.000000000000000000, 0.8123785825603968558, 1.000000000000000000),
 ( 1.000000000000000000, 0.8190671539788806355, 1.000000000000000000),
 ( 1.000000000000000000, 0.8192352254834333047, 1.000000000000000000),
 ( 1.000000000000000000, 0.8126129677212012847, 1.000000000000000000),
 ( 1.000000000000000000, 0.8047712537969730073, 1.000000000000000000) ) ) 
 REPRESENTATION_ITEM ( '' )  SURFACE ( )  );
#3928 = AXIS2_PLACEMENT_3D ( 'NONE', #14872, #14970, #7329 ) ;
#3929 = CARTESIAN_POINT ( 'NONE',  ( -154.9999999999999716, -14.99999999999999645, -15.79999999999999538 ) ) ;
#3930 = DIRECTION ( 'NONE',  ( -0.000000000000000000, -1.000000000000000000, 8.673617379884035472E-16 ) ) ;
#3931 = CARTESIAN_POINT ( 'NONE',  ( 48.02776887271745210, 65.39948385550239607, -5.992620115222778487 ) ) ;
#3932 = CARTESIAN_POINT ( 'NONE',  ( -20.63749999999999929, 0.000000000000000000, 0.000000000000000000 ) ) ;
#3933 = VECTOR ( 'NONE', #18263, 1000.000000000000114 ) ;
#3934 = CARTESIAN_POINT ( 'NONE',  ( 0.1397371499203167444, 1.362866705341264195, 3.499999999999999556 ) ) ;
#3935 = CARTESIAN_POINT ( 'NONE',  ( 55.69932041026404335, 49.89948385550241028, -1.875703265242203432 ) ) ;
#3936 = CARTESIAN_POINT ( 'NONE',  ( -29.99999999999999645, -40.00000000000000000, 10.00000000000000000 ) ) ;
#3937 = CARTESIAN_POINT ( 'NONE',  ( 57.36023556966787851, 47.99948385550239038, -0.02388180880522424582 ) ) ;
#3938 = CARTESIAN_POINT ( 'NONE',  ( 52.62207051974829852, 50.60051614449765367, -7.992620115222797139 ) ) ;
#3939 = LINE ( 'NONE', #17477, #5569 ) ;
#3940 = DIRECTION ( 'NONE',  ( -1.000000000000000000, -0.000000000000000000, -0.000000000000000000 ) ) ;
#3941 = ADVANCED_FACE ( 'NONE', ( #4444 ), #10404, .F. ) ;
#3942 = ORIENTED_EDGE ( 'NONE', *, *, #13805, .F. ) ;
#3943 = DIRECTION ( 'NONE',  ( -1.000000000000000000, 0.000000000000000000, 0.000000000000000000 ) ) ;
#3944 = EDGE_CURVE ( 'NONE', #13265, #15972, #12340, .T. ) ;
#3945 = LINE ( 'NONE', #2489, #8122 ) ;
#3946 = CARTESIAN_POINT ( 'NONE',  ( 44.03140696652198471, 55.80051614449765651, 4.306917132069485454 ) ) ;
#3947 = CARTESIAN_POINT ( 'NONE',  ( 6.367873360227559232, -5.773502691896263528, 0.000000000000000000 ) ) ;
#3948 = COLOUR_RGB ( '',0.8941176470588234615, 0.8941176470588234615, 0.8941176470588234615 ) ;
#3949 = DIRECTION ( 'NONE',  ( 2.191393683118470056E-17, 7.538405132783724027E-17, 1.000000000000000000 ) ) ;
#3950 = EDGE_LOOP ( 'NONE', ( #1455, #16464, #13611, #3677 ) ) ;
#3951 = CARTESIAN_POINT ( 'NONE',  ( 3.950241966888158540, -3.393956070638132871, 1.121495646998118545 ) ) ;
#3952 = CARTESIAN_POINT ( 'NONE',  ( -129.9999999999999716, -14.99999999999999645, -3.999999999999999112 ) ) ;
#3953 = CARTESIAN_POINT ( 'NONE',  ( 4.175002511812151873, 2.208363329454889445, -3.469254087858244073 ) ) ;
#3954 = CARTESIAN_POINT ( 'NONE',  ( 50.02271294988512551, 52.49948385550240459, 7.000000000000000888 ) ) ;
#3955 = DIRECTION ( 'NONE',  ( 1.000000000000000000, 0.000000000000000000, 0.000000000000000000 ) ) ;
#3956 = CARTESIAN_POINT ( 'NONE',  ( 42.39856655714566358, 46.89948385550240317, 2.493737253992119207 ) ) ;
#3957 = CARTESIAN_POINT ( 'NONE',  ( -18.00000000000000355, -19.99999999999999289, -12.00000000000000000 ) ) ;
#3958 = CARTESIAN_POINT ( 'NONE',  ( 56.65037692655921120, 51.10051614449766078, 2.184720259617097593 ) ) ;
#3959 = FACE_OUTER_BOUND ( 'NONE', #13204, .T. ) ;
#3960 = DIRECTION ( 'NONE',  ( 1.000000000000000000, 0.000000000000000000, -0.000000000000000000 ) ) ;
#3961 = ORIENTED_EDGE ( 'NONE', *, *, #14283, .F. ) ;
#3962 = VERTEX_POINT ( 'NONE', #13639 ) ;
#3963 = CARTESIAN_POINT ( 'NONE',  ( -1.000000000000000000, -14.00000000000000000, -9.000000000000001776 ) ) ;
#3964 = ORIENTED_EDGE ( 'NONE', *, *, #2815, .F. ) ;
#3965 = CARTESIAN_POINT ( 'NONE',  ( 4.055498735588912496, -1.410041617600660491, 3.568038744583366118 ) ) ;
#3966 = AXIS2_PLACEMENT_3D ( 'NONE', #14131, #2193, #6784 ) ;
#3967 = ORIENTED_EDGE ( 'NONE', *, *, #195, .T. ) ;
#3968 = FACE_OUTER_BOUND ( 'NONE', #9669, .T. ) ;
#3969 = CARTESIAN_POINT ( 'NONE',  ( 45.86712807150323812, 57.29948385550240175, -5.649768623646098220 ) ) ;
#3970 = ORIENTED_EDGE ( 'NONE', *, *, #16612, .F. ) ;
#3971 = CARTESIAN_POINT ( 'NONE',  ( -30.00000000000000000, -3.000000000000000000, 6.000000000000001776 ) ) ;
#3972 = ORIENTED_EDGE ( 'NONE', *, *, #12047, .F. ) ;
#3973 = CARTESIAN_POINT ( 'NONE',  ( 47.37792948025162332, 57.39948385550241028, -7.992620115222770494 ) ) ;
#3974 = CARTESIAN_POINT ( 'NONE',  ( 13.61000000000001009, 0.000000000000000000, 0.000000000000000000 ) ) ;
#3975 = PRODUCT_DEFINITION_SHAPE ( 'NONE', 'NONE',  #19437 ) ;
#3976 = CARTESIAN_POINT ( 'NONE',  ( 51.92680522751233951, 49.59948385550241312, -6.007379884777223289 ) ) ;
#3977 = LINE ( 'NONE', #1331, #6648 ) ;
#3978 = CARTESIAN_POINT ( 'NONE',  ( 1.249999999999997558, 0.000000000000000000, 0.000000000000000000 ) ) ;
#3979 = CARTESIAN_POINT ( 'NONE',  ( 50.02271294988505446, 46.50051614449766646, -8.000000000000001776 ) ) ;
#3980 = CARTESIAN_POINT ( 'NONE',  ( 50.02271294988511841, 64.49948385550239038, 6.000000000000000888 ) ) ;
#3981 = CIRCLE ( 'NONE', #1787, 3.800000000000000266 ) ;
#3982 = CARTESIAN_POINT ( 'NONE',  ( 2.804994570502171047, 3.229033611042449792, -3.526374918436834704 ) ) ;
#3983 = AXIS2_PLACEMENT_3D ( 'NONE', #13808, #9110, #18049 ) ;
#3984 = FACE_BOUND ( 'NONE', #2990, .T. ) ;
#3985 = ADVANCED_FACE ( 'NONE', ( #16500 ), #16753, .T. ) ;
#3986 = ORIENTED_EDGE ( 'NONE', *, *, #14771, .F. ) ;
#3987 = ORIENTED_EDGE ( 'NONE', *, *, #5991, .T. ) ;
#3988 = CARTESIAN_POINT ( 'NONE',  ( -159.0000000000000000, -14.99999999999999645, 15.79999999999999893 ) ) ;
#3989 = ORIENTED_EDGE ( 'NONE', *, *, #540, .T. ) ;
#3990 = CARTESIAN_POINT ( 'NONE',  ( 45.86712807150323812, 57.29948385550240175, -5.649768623646098220 ) ) ;
#3991 = FACE_OUTER_BOUND ( 'NONE', #16059, .T. ) ;
#3992 = CIRCLE ( 'NONE', #5882, 1.000000000000000666 ) ;
#3993 = ORIENTED_EDGE ( 'NONE', *, *, #9285, .F. ) ;
#3994 = EDGE_LOOP ( 'NONE', ( #17815, #2206 ) ) ;
#3995 = CARTESIAN_POINT ( 'NONE',  ( -15.51323935927264941, -32.62297130559655045, 0.000000000000000000 ) ) ;
#3996 = AXIS2_PLACEMENT_3D ( 'NONE', #5678, #2661, #1272 ) ;
#3997 = VERTEX_POINT ( 'NONE', #121 ) ;
#3998 = CARTESIAN_POINT ( 'NONE',  ( 0.05140428708382657752, 4.819072548984005167, 1.653121499799249605 ) ) ;
#3999 = VERTEX_POINT ( 'NONE', #18072 ) ;
#4000 = CIRCLE ( 'NONE', #12439, 4.000000000000003553 ) ;
#4001 = CARTESIAN_POINT ( 'NONE',  ( 55.94051828345050836, 49.79948385550240175, -4.345558710429104465 ) ) ;
#4002 = CARTESIAN_POINT ( 'NONE',  ( -9.037824375505429941, -37.84146099840256738, 0.000000000000000000 ) ) ;
#4003 = ADVANCED_FACE ( 'NONE', ( #4635 ), #409, .F. ) ;
#4004 = CARTESIAN_POINT ( 'NONE',  ( 52.29715082351538769, 46.60051614449766078, -6.992620115222796251 ) ) ;
#4005 = CARTESIAN_POINT ( 'NONE',  ( -160.9999999999999432, -14.99999999999999645, 9.000000000000000000 ) ) ;
#4006 = CARTESIAN_POINT ( 'NONE',  ( -30.00000000000000000, -7.500000000000005329, -10.00000000000000711 ) ) ;
#4007 = AXIS2_PLACEMENT_3D ( 'NONE', #5808, #17777, #10304 ) ;
#4008 = EDGE_CURVE ( 'NONE', #7334, #15786, #12450, .T. ) ;
#4009 = ADVANCED_FACE ( 'NONE', ( #1980, #698 ), #16787, .F. ) ;
#4010 = ORIENTED_EDGE ( 'NONE', *, *, #7307, .F. ) ;
#4011 = ORIENTED_EDGE ( 'NONE', *, *, #5676, .F. ) ;
#4012 = CARTESIAN_POINT ( 'NONE',  ( 8.500000000000000000, -5.773502691896263528, 0.000000000000000000 ) ) ;
#4013 = LINE ( 'NONE', #15216, #14946 ) ;
#4014 = DIRECTION ( 'NONE',  ( 0.000000000000000000, 0.000000000000000000, -1.000000000000000000 ) ) ;
#4015 = CONTEXT_DEPENDENT_SHAPE_REPRESENTATION ( #1024, #2423 ) ;
#4016 = ORIENTED_EDGE ( 'NONE', *, *, #9681, .F. ) ;
#4017 = CARTESIAN_POINT ( 'NONE',  ( 2.000000000000000000, 1.773042676681340524, -2.059984127722458425E-15 ) ) ;
#4018 = EDGE_CURVE ( 'NONE', #4718, #4669, #18635, .T. ) ;
#4020 = EDGE_CURVE ( 'NONE', #18532, #4549, #3451, .T. ) ;
#4019 = ORIENTED_EDGE ( 'NONE', *, *, #13243, .T. ) ;
#4021 = VERTEX_POINT ( 'NONE', #6669 ) ;
#4022 = AXIS2_PLACEMENT_3D ( 'NONE', #18643, #6659, #3533 ) ;
#4023 = VECTOR ( 'NONE', #12636, 1000.000000000000000 ) ;
#4024 = EDGE_CURVE ( 'NONE', #4165, #13672, #19276, .T. ) ;
#4025 = DIRECTION ( 'NONE',  ( 2.191393683118470056E-17, 7.538405132783724027E-17, 1.000000000000000000 ) ) ;
#4026 = CARTESIAN_POINT ( 'NONE',  ( 6.244297270353404095, 0.9889575675955796230, -5.105276777067857097 ) ) ;
#4027 = CARTESIAN_POINT ( 'NONE',  ( 55.69932041026405045, 51.10051614449766078, 1.875703265242156359 ) ) ;
#4028 = LINE ( 'NONE', #9891, #9519 ) ;
#4029 = LINE ( 'NONE', #14207, #7447 ) ;
#4030 = CARTESIAN_POINT ( 'NONE',  ( 55.71335778527780747, 52.09948385550241312, 1.832500667257165983 ) ) ;
#4031 = COLOUR_RGB ( '',0.8941176470588234615, 0.8941176470588234615, 0.8941176470588234615 ) ;
#4032 = CARTESIAN_POINT ( 'NONE',  ( 0.000000000000000000, 0.000000000000000000, -0.8000000000000000444 ) ) ;
#4033 = CARTESIAN_POINT ( 'NONE',  ( 50.02271294988512551, 46.49948385550240459, 7.000000000000000888 ) ) ;
#4034 = CARTESIAN_POINT ( 'NONE',  ( 58.41169779390614281, 47.00051614449766646, 0.02388180880515032231 ) ) ;
#4035 = DIRECTION ( 'NONE',  ( 1.000000000000000000, 0.000000000000000000, 0.000000000000000000 ) ) ;
#4036 = DIRECTION ( 'NONE',  ( -0.000000000000000000, 0.000000000000000000, -1.000000000000000000 ) ) ;
#4037 = CIRCLE ( 'NONE', #10292, 1.000000000000000444 ) ;
#4038 = VECTOR ( 'NONE', #17718, 1000.000000000000000 ) ;
#4039 = SHAPE_REPRESENTATION ( 'reel holder bar', ( #10359 ), #3416 ) ;
#4040 = ORIENTED_EDGE ( 'NONE', *, *, #15055, .F. ) ;
#4041 = FACE_BOUND ( 'NONE', #13319, .T. ) ;
#4042 = DIRECTION ( 'NONE',  ( 1.000000000000000000, 0.000000000000000000, 0.000000000000000000 ) ) ;
#4043 =( GEOMETRIC_REPRESENTATION_CONTEXT ( 3 ) GLOBAL_UNCERTAINTY_ASSIGNED_CONTEXT ( ( #3239 ) ) GLOBAL_UNIT_ASSIGNED_CONTEXT ( ( #11941, #8995, #9095 ) ) REPRESENTATION_CONTEXT ( 'NONE', 'WORKASPACE' ) );
#4044 = CARTESIAN_POINT ( 'NONE',  ( 43.34962307344078880, 54.10051614449766788, -2.184720259617096705 ) ) ;
#4045 = CARTESIAN_POINT ( 'NONE',  ( 6.534838248920899595, -2.951765777552420644, -5.112608298763837489 ) ) ;
#4046 = CARTESIAN_POINT ( 'NONE',  ( -154.9999999999999716, -14.99999999999999645, -15.79999999999999893 ) ) ;
#4047 = ORIENTED_EDGE ( 'NONE', *, *, #12958, .T. ) ;
#4048 = CIRCLE ( 'NONE', #14690, 2.000000000000000000 ) ;
#4049 = CARTESIAN_POINT ( 'NONE',  ( 0.4465819873852002742, 2.886751345948125547, 4.999999999999999112 ) ) ;
#4050 = EDGE_CURVE ( 'NONE', #1649, #1056, #16119, .T. ) ;
#4051 = AXIS2_PLACEMENT_3D ( 'NONE', #6606, #2310, #5229 ) ;
#4052 = CARTESIAN_POINT ( 'NONE',  ( 3.472371940585993855, 2.614027278893175321, -3.320322319201766792 ) ) ;
#4053 = CARTESIAN_POINT ( 'NONE',  ( 43.34962307344081012, 52.89948385550240317, 2.184720259617164650 ) ) ;
#4054 = CARTESIAN_POINT ( 'NONE',  ( -154.8532481325730998, -18.99730707969838761, 17.00000000000000000 ) ) ;
#4055 = CARTESIAN_POINT ( 'NONE',  ( 52.62207051974839089, 46.39948385550240317, 7.992620115222770494 ) ) ;
#4056 = ADVANCED_FACE ( 'NONE', ( #9219, #3353 ), #4911, .F. ) ;
#4057 = CARTESIAN_POINT ( 'NONE',  ( 45.86712807150329496, 45.70051614449766220, 5.649768623646139964 ) ) ;
#4058 = CARTESIAN_POINT ( 'NONE',  ( 49.99999999999997158, 45.00000000000001421, -7.499999999999998224 ) ) ;
#4059 = FACE_OUTER_BOUND ( 'NONE', #13752, .T. ) ;
#4060 = VERTEX_POINT ( 'NONE', #15593 ) ;
#4061 = ORIENTED_EDGE ( 'NONE', *, *, #11180, .T. ) ;
#4062 = CARTESIAN_POINT ( 'NONE',  ( -30.00000000000000000, 3.000000000000000000, 5.999999999999998224 ) ) ;
#4063 = EDGE_LOOP ( 'NONE', ( #8392, #17053 ) ) ;
#4064 = AXIS2_PLACEMENT_3D ( 'NONE', #8932, #1199, #1099 ) ;
#4065 = AXIS2_PLACEMENT_3D ( 'NONE', #584, #18259, #12542 ) ;
#4066 = CARTESIAN_POINT ( 'NONE',  ( 4.180345472528542494, 2.086001522971430600, 3.570468649087212398 ) ) ;
#4067 = EDGE_LOOP ( 'NONE', ( #1661, #8705, #14473, #11743 ) ) ;
#4068 = CARTESIAN_POINT ( 'NONE',  ( 4.211140560182196957, 2.431303136016536470, -3.745885042887433514 ) ) ;
#4069 = CARTESIAN_POINT ( 'NONE',  ( 54.13287192849676188, 60.29948385550240886, 5.649768623646098220 ) ) ;
#4070 = ORIENTED_EDGE ( 'NONE', *, *, #7617, .F. ) ;
#4071 = AXIS2_PLACEMENT_3D ( 'NONE', #11128, #3249, #9014 ) ;
#4072 = DIRECTION ( 'NONE',  ( -1.000000000000000000, 0.000000000000000000, 0.000000000000000000 ) ) ;
#4073 = ORIENTED_EDGE ( 'NONE', *, *, #3526, .T. ) ;
#4074 = CARTESIAN_POINT ( 'NONE',  ( 52.57664461997811856, 61.59948385550240602, -8.007379884777229506 ) ) ;
#4075 = DIRECTION ( 'NONE',  ( 1.000000000000000000, -0.000000000000000000, -0.000000000000000000 ) ) ;
#4076 = EDGE_CURVE ( 'NONE', #11041, #10947, #145, .T. ) ;
#4077 = CARTESIAN_POINT ( 'NONE',  ( 51.92680522751233951, 47.59948385550239891, -6.007379884777223289 ) ) ;
#4078 = DIRECTION ( 'NONE',  ( -0.000000000000000000, -0.000000000000000000, -1.000000000000000000 ) ) ;
#4079 = CARTESIAN_POINT ( 'NONE',  ( 0.000000000000000000, 0.000000000000000000, 5.000000000000000000 ) ) ;
#4080 = CARTESIAN_POINT ( 'NONE',  ( 45.90387839640208512, 64.30051614449766362, -5.676469297603124353 ) ) ;
#4081 = B_SPLINE_CURVE_WITH_KNOTS ( 'NONE', 3,
 ( #7936, #6008, #13825, #18168, #405, #4725 ),
 .UNSPECIFIED., .F., .F.,
 ( 4, 2, 4 ),
 ( 0.000000000000000000, 0.002086519881787260184, 0.004173039763574520368 ),
 .UNSPECIFIED. ) ;
#4082 = CARTESIAN_POINT ( 'NONE',  ( 48.07319477248762496, 46.40051614449765793, -6.007379884777208190 ) ) ;
#4083 = CARTESIAN_POINT ( 'NONE',  ( 1.925929944387235853E-31, 15.00000000000001599, -9.999999999999998224 ) ) ;
#4084 = AXIS2_PLACEMENT_3D ( 'NONE', #18600, #13954, #7981 ) ;
#4085 = DIRECTION ( 'NONE',  ( 0.000000000000000000, 0.000000000000000000, 1.000000000000000000 ) ) ;
#4086 = ORIENTED_EDGE ( 'NONE', *, *, #7359, .F. ) ;
#4087 = ORIENTED_EDGE ( 'NONE', *, *, #4050, .F. ) ;
#4088 = CARTESIAN_POINT ( 'NONE',  ( -1.935715396507168721E-15, 2.686816014504566752, 2.346298152288372130 ) ) ;
#4089 = VERTEX_POINT ( 'NONE', #13830 ) ;
#4090 = CARTESIAN_POINT ( 'NONE',  ( 47.70284917648453415, 57.39948385550241028, -6.992620115222774047 ) ) ;
#4091 = DIRECTION ( 'NONE',  ( -0.000000000000000000, 0.000000000000000000, -1.000000000000000000 ) ) ;
#4092 = VERTEX_POINT ( 'NONE', #18267 ) ;
#4093 = ORIENTED_EDGE ( 'NONE', *, *, #8697, .F. ) ;
#4094 = DIRECTION ( 'NONE',  ( -0.6691306063588624564, 0.7431448254773903583, 0.000000000000000000 ) ) ;
#4095 = ORIENTED_EDGE ( 'NONE', *, *, #16710, .F. ) ;
#4096 = CIRCLE ( 'NONE', #10333, 1.000000000000000000 ) ;
#4097 = LINE ( 'NONE', #2444, #1302 ) ;
#4098 = AXIS2_PLACEMENT_3D ( 'NONE', #2989, #16516, #5825 ) ;
#4099 = ORIENTED_EDGE ( 'NONE', *, *, #10632, .T. ) ;
#4100 = CARTESIAN_POINT ( 'NONE',  ( 1.000000000000000000, -14.00000000000000000, 8.999999999999998224 ) ) ;
#4101 = CARTESIAN_POINT ( 'NONE',  ( 44.05948171654949874, 48.79948385550238754, 4.345558710429105354 ) ) ;
#4102 = CARTESIAN_POINT ( 'NONE',  ( -9.999999999999996447, 25.00000000000001776, 15.00000000000000000 ) ) ;
#4103 = VECTOR ( 'NONE', #18373, 1000.000000000000000 ) ;
#4104 = CARTESIAN_POINT ( 'NONE',  ( 56.66441430157294690, 50.90051614449766504, -2.141517661632166281 ) ) ;
#4105 = FACE_OUTER_BOUND ( 'NONE', #8096, .T. ) ;
#4106 = PRESENTATION_STYLE_ASSIGNMENT (( #18832 ) ) ;
#4107 = CARTESIAN_POINT ( 'NONE',  ( 19.30627432446651426, -25.22185519795840136, 9.000000000000000000 ) ) ;
#4108 = VECTOR ( 'NONE', #4801, 1000.000000000000000 ) ;
#4109 = VERTEX_POINT ( 'NONE', #16888 ) ;
#4110 = EDGE_LOOP ( 'NONE', ( #4990, #9146, #8929, #1507, #4681 ) ) ;
#4111 = CARTESIAN_POINT ( 'NONE',  ( 4.050536630291690976, 3.778525289263159781, 0.5912575323401418892 ) ) ;
#4112 = SURFACE_SIDE_STYLE ('',( #1268 ) ) ;
#4113 = CYLINDRICAL_SURFACE ( 'NONE', #3996, 2.649999999999985700 ) ;
#4114 = CARTESIAN_POINT ( 'NONE',  ( 75.00000000000001421, -7.499999999999971578, -20.00000000000000000 ) ) ;
#4115 = ORIENTED_EDGE ( 'NONE', *, *, #19379, .F. ) ;
#4116 = CARTESIAN_POINT ( 'NONE',  ( 6.323279575526388641, 5.335162385629701909, 0.7592276814629709270 ) ) ;
#4117 = ORIENTED_EDGE ( 'NONE', *, *, #17810, .T. ) ;
#4118 = ORIENTED_EDGE ( 'NONE', *, *, #4188, .F. ) ;
#4119 = EDGE_CURVE ( 'NONE', #7193, #15477, #17370, .T. ) ;
#4120 = CYLINDRICAL_SURFACE ( 'NONE', #12535, 20.00000000000000000 ) ;
#4121 = CARTESIAN_POINT ( 'NONE',  ( -16.79901371501580698, -30.85325472854621864, 9.000000000000000000 ) ) ;
#4122 = AXIS2_PLACEMENT_3D ( 'NONE', #7420, #3017, #1736 ) ;
#4123 = CARTESIAN_POINT ( 'NONE',  ( 43.69122665457040000, 52.00051614449766646, -0.02388180880515696977 ) ) ;
#4124 = CARTESIAN_POINT ( 'NONE',  ( 2.449293598294706513E-15, -20.00000000000000000, 9.000000000000000000 ) ) ;
#4125 = EDGE_CURVE ( 'NONE', #4747, #5816, #8135, .T. ) ;
#4126 = CARTESIAN_POINT ( 'NONE',  ( -17.79870116617242459, -29.12174527145394265, 9.000000000000000000 ) ) ;
#4127 = CIRCLE ( 'NONE', #15087, 1.000000000000001110 ) ;
#4128 = CARTESIAN_POINT ( 'NONE',  ( 44.91013252490152752, 50.79948385550240175, 3.727524721679198461 ) ) ;
#4129 = DIRECTION ( 'NONE',  ( -0.000000000000000000, -0.000000000000000000, -1.000000000000000000 ) ) ;
#4130 = CARTESIAN_POINT ( 'NONE',  ( 57.36023556966787851, 45.99948385550238328, -0.02388180880522424582 ) ) ;
#4131 = CARTESIAN_POINT ( 'NONE',  ( 49.97728705011495265, 45.50051614449766646, 8.000000000000001776 ) ) ;
#4132 = ADVANCED_FACE ( 'NONE', ( #13733 ), #4822, .F. ) ;
#4133 = EDGE_CURVE ( 'NONE', #13670, #1462, #2071, .T. ) ;
#4134 = ORIENTED_EDGE ( 'NONE', *, *, #13706, .F. ) ;
#4135 = CARTESIAN_POINT ( 'NONE',  ( -8.134732861516020819, -1.729090847147989773, -9.000000000000000000 ) ) ;
#4136 =( NAMED_UNIT ( * ) PLANE_ANGLE_UNIT ( ) SI_UNIT ( $, .RADIAN. ) );
#4137 = EDGE_CURVE ( 'NONE', #6443, #16399, #12556, .T. ) ;
#4138 = SHAPE_DEFINITION_REPRESENTATION ( #1471, #18081 ) ;
#4139 = ORIENTED_EDGE ( 'NONE', *, *, #5848, .T. ) ;
#4140 = LINE ( 'NONE', #10106, #2374 ) ;
#4141 = PRODUCT_DEFINITION_SHAPE ( 'NONE', 'NONE',  #160 ) ;
#4142 = VECTOR ( 'NONE', #3218, 1000.000000000000000 ) ;
#4143 = CARTESIAN_POINT ( 'NONE',  ( 0.1717365941144614327, -6.008326913195983998, 0.000000000000000000 ) ) ;
#4144 = EDGE_CURVE ( 'NONE', #7961, #11553, #15209, .T. ) ;
#4145 = CARTESIAN_POINT ( 'NONE',  ( 0.4472135954999577612, 6.613092715395707467E-16, -5.400000000000000355 ) ) ;
#4146 = EDGE_CURVE ( 'NONE', #9743, #15873, #3633, .T. ) ;
#4147 = DIRECTION ( 'NONE',  ( 0.000000000000000000, 0.000000000000000000, -1.000000000000000000 ) ) ;
#4148 = VERTEX_POINT ( 'NONE', #3259 ) ;
#4149 = LINE ( 'NONE', #10113, #12965 ) ;
#4150 = CYLINDRICAL_SURFACE ( 'NONE', #3067, 1.000000000000000000 ) ;
#4151 = CARTESIAN_POINT ( 'NONE',  ( 54.13287192849676188, 54.29948385550240886, 5.649768623646098220 ) ) ;
#4152 = CIRCLE ( 'NONE', #9779, 0.5999999999999980904 ) ;
#4153 = FACE_OUTER_BOUND ( 'NONE', #6701, .T. ) ;
#4154 = CARTESIAN_POINT ( 'NONE',  ( 43.20883090819742023, 64.20051614449766930, -4.963592699178938972 ) ) ;
#4155 = PRESENTATION_STYLE_ASSIGNMENT (( #15821 ) ) ;
#4156 = CARTESIAN_POINT ( 'NONE',  ( 43.33558569842706021, 45.90051614449765793, 2.141517661632167169 ) ) ;
#4157 = DIRECTION ( 'NONE',  ( -1.000000000000000000, -0.000000000000000000, -0.000000000000000000 ) ) ;
#4158 = ORIENTED_EDGE ( 'NONE', *, *, #18214, .F. ) ;
#4159 = ORIENTED_EDGE ( 'NONE', *, *, #19179, .T. ) ;
#4160 = DIRECTION ( 'NONE',  ( 1.000000000000000000, 0.000000000000000000, 0.000000000000000000 ) ) ;
#4161 = ORIENTED_EDGE ( 'NONE', *, *, #12082, .F. ) ;
#4162 = FACE_OUTER_BOUND ( 'NONE', #4530, .T. ) ;
#4163 = ORIENTED_EDGE ( 'NONE', *, *, #6041, .F. ) ;
#4164 = LINE ( 'NONE', #11498, #974 ) ;
#4165 = VERTEX_POINT ( 'NONE', #1786 ) ;
#4166 = CARTESIAN_POINT ( 'NONE',  ( 0.4465819873849485311, -2.886751345948517677, -5.000000000000000000 ) ) ;
#4167 = ORIENTED_EDGE ( 'NONE', *, *, #14666, .T. ) ;
#4168 = CARTESIAN_POINT ( 'NONE',  ( 52.62207051974839089, 56.39948385550241028, 7.992620115222770494 ) ) ;
#4169 = DIRECTION ( 'NONE',  ( 0.000000000000000000, 0.000000000000000000, 1.000000000000000000 ) ) ;
#4170 = CARTESIAN_POINT ( 'NONE',  ( 51.97223112728254790, 48.39948385550240317, 5.992620115222778487 ) ) ;
#4171 = ADVANCED_FACE ( 'NONE', ( #3835 ), #11163, .F. ) ;
#4172 = LINE ( 'NONE', #2626, #16378 ) ;
#4173 = DIRECTION ( 'NONE',  ( 0.000000000000000000, 0.000000000000000000, 1.000000000000000000 ) ) ;
#4174 = CARTESIAN_POINT ( 'NONE',  ( 42.39856655714564226, 48.10051614449766078, -2.493737253992044156 ) ) ;
#4175 = CARTESIAN_POINT ( 'NONE',  ( 46.49166364869456913, 46.30051614449766362, -4.867452303228181343 ) ) ;
#4176 = CARTESIAN_POINT ( 'NONE',  ( 1.000000000000000444, -15.10102051443364246, 9.000000000000000000 ) ) ;
#4177 = DIRECTION ( 'NONE',  ( 1.224646799147353207E-16, 1.000000000000000000, 0.000000000000000000 ) ) ;
#4178 = ORIENTED_EDGE ( 'NONE', *, *, #7820, .T. ) ;
#4179 = VERTEX_POINT ( 'NONE', #9797 ) ;
#4180 = DIRECTION ( 'NONE',  ( 1.000000000000000000, 0.000000000000000000, 0.000000000000000000 ) ) ;
#4181 = ORIENTED_EDGE ( 'NONE', *, *, #1630, .T. ) ;
#4182 = ADVANCED_FACE ( 'NONE', ( #15987 ), #13137, .F. ) ;
#4183 = CARTESIAN_POINT ( 'NONE',  ( 47.74827507625478518, 56.59948385550238470, 7.007379884777227730 ) ) ;
#4184 = CYLINDRICAL_SURFACE ( 'NONE', #17508, 2.100000000000000089 ) ;
#4185 = ORIENTED_EDGE ( 'NONE', *, *, #6921, .T. ) ;
#4186 = EDGE_LOOP ( 'NONE', ( #530, #16037, #5136, #18918, #10560 ) ) ;
#4187 = LINE ( 'NONE', #13008, #15668 ) ;
#4188 = EDGE_CURVE ( 'NONE', #3704, #9229, #18945, .T. ) ;
#4189 = DIRECTION ( 'NONE',  ( -1.000000000000000000, 0.000000000000000000, 0.000000000000000000 ) ) ;
#4190 = ORIENTED_EDGE ( 'NONE', *, *, #3531, .T. ) ;
#4191 = CARTESIAN_POINT ( 'NONE',  ( -20.63749999999999929, 5.419062086227038392E-16, 4.424999999999999822 ) ) ;
#4192 = VERTEX_POINT ( 'NONE', #5393 ) ;
#4193 = CARTESIAN_POINT ( 'NONE',  ( 0.02448733951239481094, 4.877042772274728044, -3.751161874094022242 ) ) ;
#4194 = CARTESIAN_POINT ( 'NONE',  ( 52.29715082351547295, 52.39948385550241738, 6.992620115222774047 ) ) ;
#4195 = PLANE ( 'NONE',  #6785 ) ;
#4196 = CARTESIAN_POINT ( 'NONE',  ( 42.63976443033212860, 46.00051614449766646, -0.02388180880514948964 ) ) ;
#4197 = CARTESIAN_POINT ( 'NONE',  ( -11.75570504584948139, -3.819660112501066518, -9.000000000000000000 ) ) ;
#4198 = LINE ( 'NONE', #11731, #5821 ) ;
#4199 = CARTESIAN_POINT ( 'NONE',  ( 2.449293598294706513E-15, -20.00000000000000000, -9.000000000000000000 ) ) ;
#4200 = AXIS2_PLACEMENT_3D ( 'NONE', #17803, #234, #3096 ) ;
#4201 = VERTEX_POINT ( 'NONE', #15890 ) ;
#4202 = VERTEX_POINT ( 'NONE', #17276 ) ;
#4203 = CARTESIAN_POINT ( 'NONE',  ( 3.098410542199072637, -7.060458129626440815, -1.000000000000000000 ) ) ;
#4204 = PRESENTATION_STYLE_ASSIGNMENT (( #5973 ) ) ;
#4205 = CIRCLE ( 'NONE', #8886, 8.105212085995399107 ) ;
#4206 = CARTESIAN_POINT ( 'NONE',  ( 6.534838248920897819, 2.951765777552411318, -5.112608298763837489 ) ) ;
#4207 = DIRECTION ( 'NONE',  ( 0.000000000000000000, 1.000000000000000000, -1.224646799147353207E-16 ) ) ;
#4208 = ORIENTED_EDGE ( 'NONE', *, *, #18395, .F. ) ;
#4209 = CARTESIAN_POINT ( 'NONE',  ( 6.095473853218515536, 3.806361898857873793, 3.407187799183811983 ) ) ;
#4210 = ORIENTED_EDGE ( 'NONE', *, *, #6749, .F. ) ;
#4211 = ORIENTED_EDGE ( 'NONE', *, *, #3537, .F. ) ;
#4212 = CARTESIAN_POINT ( 'NONE',  ( 4.688877333453707941, -18.97314589549297281, 9.999999999999998224 ) ) ;
#4213 = VECTOR ( 'NONE', #2474, 1000.000000000000000 ) ;
#4214 = CARTESIAN_POINT ( 'NONE',  ( 46.49166364869456913, 48.30051614449765651, -4.867452303228181343 ) ) ;
#4215 = CARTESIAN_POINT ( 'NONE',  ( 0.9183817310753817909, -24.91493387504115020, 9.000000000000000000 ) ) ;
#4216 =( NAMED_UNIT ( * ) PLANE_ANGLE_UNIT ( ) SI_UNIT ( $, .RADIAN. ) );
#4217 = CARTESIAN_POINT ( 'NONE',  ( 56.30877334542961421, 47.99948385550239038, -0.02388180880520959434 ) ) ;
#4218 = CARTESIAN_POINT ( 'NONE',  ( 4.898587196589413026E-15, -40.00000000000000000, -9.000000000000000000 ) ) ;
#4219 = CARTESIAN_POINT ( 'NONE',  ( 47.70284917648453415, 53.39948385550238186, -6.992620115222774047 ) ) ;
#4220 = CARTESIAN_POINT ( 'NONE',  ( 52.57664461997821093, 49.40051614449766504, 8.007379884777206414 ) ) ;
#4221 = CARTESIAN_POINT ( 'NONE',  ( 4.175813232069148562, -2.061359961916374051, -3.570380186727397653 ) ) ;
#4222 = ORIENTED_EDGE ( 'NONE', *, *, #6179, .T. ) ;
#4223 = DIRECTION ( 'NONE',  ( 1.000000000000000000, 0.000000000000000000, 0.000000000000000000 ) ) ;
#4224 = EDGE_CURVE ( 'NONE', #2892, #6443, #793, .T. ) ;
#4225 = SHAPE_DEFINITION_REPRESENTATION ( #4141, #1297 ) ;
#4226 = AXIS2_PLACEMENT_3D ( 'NONE', #13829, #7756, #315 ) ;
#4227 = EDGE_LOOP ( 'NONE', ( #7212, #14533, #8791, #5951 ) ) ;
#4228 = AXIS2_PLACEMENT_3D ( 'NONE', #18151, #3332, #15470 ) ;
#4229 = EDGE_CURVE ( 'NONE', #402, #17786, #9698, .T. ) ;
#4230 = CARTESIAN_POINT ( 'NONE',  ( 0.1410422978106145031, -4.700232962125109104, -3.687027686973628704 ) ) ;
#4231 = DIRECTION ( 'NONE',  ( 1.000000000000000000, 0.000000000000000000, 0.000000000000000000 ) ) ;
#4232 = EDGE_CURVE ( 'NONE', #12513, #10379, #7026, .T. ) ;
#4233 = DIRECTION ( 'NONE',  ( -0.000000000000000000, -0.000000000000000000, 1.000000000000000000 ) ) ;
#4234 = CARTESIAN_POINT ( 'NONE',  ( -16.79901371501587803, -9.146745271453902149, 9.000000000000000000 ) ) ;
#4235 = CARTESIAN_POINT ( 'NONE',  ( -154.8426517387881347, -18.99690399242885874, -15.00000000000000000 ) ) ;
#4236 = DIRECTION ( 'NONE',  ( 0.000000000000000000, 0.000000000000000000, -1.000000000000000000 ) ) ;
#4237 = EDGE_CURVE ( 'NONE', #248, #17308, #4028, .T. ) ;
#4238 = CYLINDRICAL_SURFACE ( 'NONE', #3695, 8.000000000000007105 ) ;
#4239 = CARTESIAN_POINT ( 'NONE',  ( 43.33558569842703179, 55.09948385550241312, -2.141517661632099223 ) ) ;
#4240 = ADVANCED_FACE ( 'NONE', ( #12842 ), #18851, .F. ) ;
#4241 = DIRECTION ( 'NONE',  ( 1.000000000000000000, 0.000000000000000000, 0.000000000000000000 ) ) ;
#4242 = CARTESIAN_POINT ( 'NONE',  ( 54.68390685589033495, 45.69948385550240033, -6.485486291978119766 ) ) ;
#4243 = FACE_OUTER_BOUND ( 'NONE', #18627, .T. ) ;
#4244 = CARTESIAN_POINT ( 'NONE',  ( 43.34962307344078880, 48.10051614449766078, -2.184720259617096705 ) ) ;
#4245 = CARTESIAN_POINT ( 'NONE',  ( 0.000000000000000000, 0.000000000000000000, 3.469446951953614189E-15 ) ) ;
#4246 = VECTOR ( 'NONE', #19233, 1000.000000000000000 ) ;
#4248 = VERTEX_POINT ( 'NONE', #2373 ) ;
#4247 = ADVANCED_FACE ( 'NONE', ( #11558 ), #11458, .F. ) ;
#4249 = EDGE_CURVE ( 'NONE', #12819, #12668, #11364, .T. ) ;
#4250 = EDGE_LOOP ( 'NONE', ( #4254, #3383, #7149, #19103 ) ) ;
#4251 = CARTESIAN_POINT ( 'NONE',  ( -14.00000000000000000, 15.00000000000001599, 9.000000000000000000 ) ) ;
#4252 = ORIENTED_EDGE ( 'NONE', *, *, #5602, .T. ) ;
#4253 = CARTESIAN_POINT ( 'NONE',  ( 1.150000000000001688, 0.000000000000000000, 0.000000000000000000 ) ) ;
#4254 = ORIENTED_EDGE ( 'NONE', *, *, #6763, .T. ) ;
#4255 = CARTESIAN_POINT ( 'NONE',  ( 5.991014884144048480, 4.330127018922193649, -2.499999999999998668 ) ) ;
#4256 = EDGE_CURVE ( 'NONE', #4327, #16340, #16088, .T. ) ;
#4257 = ORIENTED_EDGE ( 'NONE', *, *, #10349, .T. ) ;
#4258 = EDGE_CURVE ( 'NONE', #16158, #13265, #885, .T. ) ;
#4259 = DIRECTION ( 'NONE',  ( -9.710251638871371392E-17, -5.969973981896233748E-17, -1.000000000000000000 ) ) ;
#4260 = EDGE_LOOP ( 'NONE', ( #4599, #14271, #8594 ) ) ;
#4261 = CARTESIAN_POINT ( 'NONE',  ( 54.68390685589033495, 59.69948385550240744, -6.485486291978119766 ) ) ;
#4262 = CARTESIAN_POINT ( 'NONE',  ( 62.50000000000000000, 32.50000000000001421, -9.999999999999998224 ) ) ;
#4263 = AXIS2_PLACEMENT_3D ( 'NONE', #17655, #9885, #13222 ) ;
#4264 = CARTESIAN_POINT ( 'NONE',  ( 50.02271294988511841, 58.49948385550241170, 6.000000000000000888 ) ) ;
#4265 = EDGE_CURVE ( 'NONE', #8664, #14765, #12994, .T. ) ;
#4266 = LINE ( 'NONE', #7202, #6966 ) ;
#4267 = DIRECTION ( 'NONE',  ( 0.000000000000000000, 0.000000000000000000, 1.000000000000000000 ) ) ;
#4268 = CARTESIAN_POINT ( 'NONE',  ( 57.60143344285435774, 47.10051614449766078, 2.493737253992045044 ) ) ;
#4269 = CARTESIAN_POINT ( 'NONE',  ( 48.02776887271750184, 51.60051614449766788, 5.992620115222795363 ) ) ;
#4270 = CIRCLE ( 'NONE', #18683, 5.000000000000000888 ) ;
#4271 = CARTESIAN_POINT ( 'NONE',  ( 3.973514160553462737, -2.741076955031366502, -2.383932505289870551 ) ) ;
#4272 = DIRECTION ( 'NONE',  ( 1.000000000000000000, 1.387778780781445676E-16, -0.000000000000000000 ) ) ;
#4273 = EDGE_LOOP ( 'NONE', ( #15066, #16726, #693, #14964 ) ) ;
#4274 = ORIENTED_EDGE ( 'NONE', *, *, #6301, .T. ) ;
#4275 = CARTESIAN_POINT ( 'NONE',  ( -74.99999999999997158, -1.000000000000000000, 6.000000000000001776 ) ) ;
#4276 = AXIS2_PLACEMENT_3D ( 'NONE', #11383, #15910, #1282 ) ;
#4277 = ORIENTED_EDGE ( 'NONE', *, *, #8716, .F. ) ;
#4278 = CARTESIAN_POINT ( 'NONE',  ( 45.86712807150323812, 63.29948385550240886, -5.649768623646098220 ) ) ;
#4279 = CARTESIAN_POINT ( 'NONE',  ( -154.9999999999999716, -14.99999999999999645, 15.00000000000000000 ) ) ;
#4280 = ORIENTED_EDGE ( 'NONE', *, *, #18031, .F. ) ;
#4281 = ORIENTED_EDGE ( 'NONE', *, *, #15404, .F. ) ;
#4282 = LINE ( 'NONE', #14762, #964 ) ;
#4283 = CARTESIAN_POINT ( 'NONE',  ( 55.94051828345050836, 45.79948385550240886, -4.345558710429103577 ) ) ;
#4284 = ORIENTED_EDGE ( 'NONE', *, *, #6608, .F. ) ;
#4285 = CARTESIAN_POINT ( 'NONE',  ( 0.4465819873852039379, 5.773502691896261751, 3.331019006688249527E-17 ) ) ;
#4286 = ORIENTED_EDGE ( 'NONE', *, *, #12078, .T. ) ;
#4287 = CARTESIAN_POINT ( 'NONE',  ( 3.175194142252359963, -39.74634503291702003, 9.000000000000000000 ) ) ;
#4288 = CARTESIAN_POINT ( 'NONE',  ( 56.65037692655918988, 51.89948385550241028, -2.184720259617163762 ) ) ;
#4289 = CARTESIAN_POINT ( 'NONE',  ( -62.49999999999997158, 32.50000000000001421, 15.00000000000000000 ) ) ;
#4290 = VECTOR ( 'NONE', #11440, 1000.000000000000000 ) ;
#4291 = CARTESIAN_POINT ( 'NONE',  ( 50.02271294988505446, 48.50051614449765935, -7.000000000000000888 ) ) ;
#4292 = FACE_OUTER_BOUND ( 'NONE', #9984, .T. ) ;
#4293 = ADVANCED_FACE ( 'NONE', ( #5588 ), #17570, .T. ) ;
#4294 = LINE ( 'NONE', #4396, #18550 ) ;
#4295 = CARTESIAN_POINT ( 'NONE',  ( -4.000000000000000000, 0.8730739991738342143, -3.223134629628428893 ) ) ;
#4296 = ADVANCED_FACE ( 'NONE', ( #7158, #14206 ), #8327, .F. ) ;
#4297 = PRODUCT ( 'socket head cap screw_iso_ISO 4762 M4 x 10 - 10N', 'socket head cap screw_iso_ISO 4762 M4 x 10 - 10N', '', ( #1587 ) ) ;
#4298 = ORIENTED_EDGE ( 'NONE', *, *, #1908, .F. ) ;
#4299 = EDGE_LOOP ( 'NONE', ( #18336, #9910, #12103 ) ) ;
#4300 = CARTESIAN_POINT ( 'NONE',  ( 4.071447262713887127, 2.020725942163686284, -3.499999999999999556 ) ) ;
#4301 = SURFACE_STYLE_USAGE ( .BOTH. , #11738 ) ;
#4302 = CIRCLE ( 'NONE', #7743, 20.00000000000000000 ) ;
#4303 = CARTESIAN_POINT ( 'NONE',  ( 52.29715082351547295, 48.39948385550240317, 6.992620115222774047 ) ) ;
#4304 = DIRECTION ( 'NONE',  ( 0.03086419753086420623, -0.9995235871707959241, 0.000000000000000000 ) ) ;
#4305 = ORIENTED_EDGE ( 'NONE', *, *, #5425, .F. ) ;
#4306 = AXIS2_PLACEMENT_3D ( 'NONE', #742, #6522, #12802 ) ;
#4307 = DIRECTION ( 'NONE',  ( -1.000000000000000000, 0.000000000000000000, 0.000000000000000000 ) ) ;
#4308 = ORIENTED_EDGE ( 'NONE', *, *, #18352, .F. ) ;
#4309 = ORIENTED_EDGE ( 'NONE', *, *, #9976, .T. ) ;
#4310 = CARTESIAN_POINT ( 'NONE',  ( 0.000000000000000000, 0.000000000000000000, 9.000000000000000000 ) ) ;
#4311 = CARTESIAN_POINT ( 'NONE',  ( 0.02993401039713673023, -2.688325911136453694, 2.343682934607768775 ) ) ;
#4312 = VECTOR ( 'NONE', #17880, 1000.000000000000000 ) ;
#4313 = CARTESIAN_POINT ( 'NONE',  ( 44.88205777487401349, 47.80051614449764941, 3.688883143319584779 ) ) ;
#4314 = DIRECTION ( 'NONE',  ( -0.1045284632676425907, -0.9945218953682745111, 0.000000000000000000 ) ) ;
#4315 = VECTOR ( 'NONE', #11465, 1000.000000000000000 ) ;
#4316 = LINE ( 'NONE', #10285, #11766 ) ;
#4317 = CARTESIAN_POINT ( 'NONE',  ( 53.54508667620428497, 60.29948385550240175, 4.840751629271157874 ) ) ;
#4318 = CARTESIAN_POINT ( 'NONE',  ( 3.455068668934414777, -2.624017327439094327, -3.316620875263732504 ) ) ;
#4319 = AXIS2_PLACEMENT_3D ( 'NONE', #10138, #9942, #8674 ) ;
#4320 = CARTESIAN_POINT ( 'NONE',  ( 52.25172492374522903, 49.59948385550240602, -7.007379884777225953 ) ) ;
#4321 = CARTESIAN_POINT ( 'NONE',  ( 56.81924384183006538, 44.80051614449766362, -4.924951120819380357 ) ) ;
#4322 = CARTESIAN_POINT ( 'NONE',  ( 4.151274195509678577, -2.039912954708747339, -3.533232880573492274 ) ) ;
#4323 = ORIENTED_EDGE ( 'NONE', *, *, #15886, .F. ) ;
#4324 = LINE ( 'NONE', #18063, #6498 ) ;
#4325 =( LENGTH_UNIT ( ) NAMED_UNIT ( * ) SI_UNIT ( .MILLI., .METRE. ) );
#4326 =( NAMED_UNIT ( * ) SI_UNIT ( $, .STERADIAN. ) SOLID_ANGLE_UNIT ( ) );
#4327 = VERTEX_POINT ( 'NONE', #7638 ) ;
#4328 = CARTESIAN_POINT ( 'NONE',  ( 0.1756481739660539498, -4.720212674038995360, -3.469390959564070620 ) ) ;
#4329 = CIRCLE ( 'NONE', #2470, 2.000000000000001776 ) ;
#4330 = CARTESIAN_POINT ( 'NONE',  ( -2.595115354961444076, -7.673029147243174641, -1.000000000000000000 ) ) ;
#4331 = DIRECTION ( 'NONE',  ( -0.000000000000000000, -0.000000000000000000, 1.000000000000000000 ) ) ;
#4332 = CARTESIAN_POINT ( 'NONE',  ( 2.449293598294706513E-15, -20.00000000000000000, 15.00000000000000355 ) ) ;
#4333 =( GEOMETRIC_REPRESENTATION_CONTEXT ( 3 ) GLOBAL_UNCERTAINTY_ASSIGNED_CONTEXT ( ( #7345 ) ) GLOBAL_UNIT_ASSIGNED_CONTEXT ( ( #10583, #15004, #13903 ) ) REPRESENTATION_CONTEXT ( 'NONE', 'WORKASPACE' ) );
#4334 = CARTESIAN_POINT ( 'NONE',  ( -154.9999999999999716, -23.00000000000000000, 15.00000000000000000 ) ) ;
#4335 = CARTESIAN_POINT ( 'NONE',  ( 6.367873360227555679, -2.886751345948119774, 4.999999999999999112 ) ) ;
#4336 = DIRECTION ( 'NONE',  ( 0.000000000000000000, 0.000000000000000000, -1.000000000000000000 ) ) ;
#4337 = CARTESIAN_POINT ( 'NONE',  ( 57.36023556966787851, 53.99948385550239038, -0.02388180880522424582 ) ) ;
#4338 = CARTESIAN_POINT ( 'NONE',  ( 0.000000000000000000, 0.000000000000000000, 0.000000000000000000 ) ) ;
#4339 = CARTESIAN_POINT ( 'NONE',  ( 47.37792948025162332, 55.39948385550240317, -7.992620115222770494 ) ) ;
#4340 = PLANE ( 'NONE',  #4442 ) ;
#4341 = CARTESIAN_POINT ( 'NONE',  ( 55.96859303347802239, 48.80051614449766362, -4.306917132069484566 ) ) ;
#4342 = AXIS2_PLACEMENT_3D ( 'NONE', #6725, #5158, #8201 ) ;
#4343 = CARTESIAN_POINT ( 'NONE',  ( -16.32050807568879236, -10.00000000000004263, 9.000000000000000000 ) ) ;
#4344 = ORIENTED_EDGE ( 'NONE', *, *, #14162, .F. ) ;
#4345 = PRESENTATION_LAYER_ASSIGNMENT (  '', '', ( #6534 ) ) ;
#4346 = ORIENTED_EDGE ( 'NONE', *, *, #16482, .T. ) ;
#4347 = PLANE ( 'NONE',  #14691 ) ;
#4348 = ORIENTED_EDGE ( 'NONE', *, *, #3642, .F. ) ;
#4349 = LINE ( 'NONE', #2987, #10915 ) ;
#4350 = EDGE_CURVE ( 'NONE', #7750, #15438, #8291, .T. ) ;
#4351 = ORIENTED_EDGE ( 'NONE', *, *, #11908, .F. ) ;
#4352 = CARTESIAN_POINT ( 'NONE',  ( 14.86289650954772590, -6.617387872822656725, -9.000000000000000000 ) ) ;
#4353 = AXIS2_PLACEMENT_3D ( 'NONE', #7604, #17635, #7218 ) ;
#4354 = VECTOR ( 'NONE', #17310, 1000.000000000000000 ) ;
#4355 = ORIENTED_EDGE ( 'NONE', *, *, #14909, .T. ) ;
#4356 = DIRECTION ( 'NONE',  ( -0.000000000000000000, -0.000000000000000000, 1.000000000000000000 ) ) ;
#4357 = ORIENTED_EDGE ( 'NONE', *, *, #12511, .F. ) ;
#4358 = LINE ( 'NONE', #3192, #4605 ) ;
#4359 = CARTESIAN_POINT ( 'NONE',  ( 2.449293598294706513E-15, -20.00000000000000000, -9.000000000000000000 ) ) ;
#4360 = EDGE_CURVE ( 'NONE', #1080, #13316, #7668, .T. ) ;
#4361 = CARTESIAN_POINT ( 'NONE',  ( 55.08986747509847248, 59.79948385550240175, -3.727524721679197572 ) ) ;
#4363 = ADVANCED_FACE ( 'NONE', ( #1470, #7449 ), #5690, .T. ) ;
#4362 = FACE_OUTER_BOUND ( 'NONE', #3722, .T. ) ;
#4364 = FACE_OUTER_BOUND ( 'NONE', #302, .T. ) ;
#4365 = AXIS2_PLACEMENT_3D ( 'NONE', #12854, #2383, #17380 ) ;
#4366 = CARTESIAN_POINT ( 'NONE',  ( 42.38452918213190657, 51.90051614449765793, 2.450534656007115508 ) ) ;
#4367 = CARTESIAN_POINT ( 'NONE',  ( 50.02271294988506156, 48.50051614449765935, -6.000000000000000888 ) ) ;
#4368 = EDGE_CURVE ( 'NONE', #7529, #7505, #9837, .T. ) ;
#4369 = CARTESIAN_POINT ( 'NONE',  ( 4.175813232069150338, -4.122719923832746325, 2.362127131240695889E-16 ) ) ;
#4370 = CYLINDRICAL_SURFACE ( 'NONE', #16297, 1.000000000000000000 ) ;
#4371 = AXIS2_PLACEMENT_3D ( 'NONE', #16322, #5727, #8948 ) ;
#4372 = ORIENTED_EDGE ( 'NONE', *, *, #3275, .F. ) ;
#4373 = EDGE_CURVE ( 'NONE', #1569, #6843, #5468, .T. ) ;
#4374 = CIRCLE ( 'NONE', #15323, 4.000000000000003553 ) ;
#4375 = ADVANCED_FACE ( 'NONE', ( #10572 ), #2860, .T. ) ;
#4376 = ORIENTED_EDGE ( 'NONE', *, *, #11157, .F. ) ;
#4377 = DIRECTION ( 'NONE',  ( -1.000000000000000000, 0.000000000000000000, 0.000000000000000000 ) ) ;
#4378 = ORIENTED_EDGE ( 'NONE', *, *, #9501, .F. ) ;
#4379 = CARTESIAN_POINT ( 'NONE',  ( 43.33558569842703179, 65.09948385550239891, -2.141517661632099223 ) ) ;
#4380 = DIRECTION ( 'NONE',  ( -0.9999670257950099561, -0.008120795692649453515, 0.000000000000000000 ) ) ;
#4381 = CIRCLE ( 'NONE', #15970, 0.9999999999999980016 ) ;
#4382 = EDGE_LOOP ( 'NONE', ( #17344, #13774 ) ) ;
#4383 = CARTESIAN_POINT ( 'NONE',  ( -17.32050807568872841, -30.00000000000008171, -9.000000000000000000 ) ) ;
#4384 = CARTESIAN_POINT ( 'NONE',  ( 50.02271294988512551, 48.49948385550240459, 7.000000000000000888 ) ) ;
#4385 = ORIENTED_EDGE ( 'NONE', *, *, #12987, .T. ) ;
#4386 = CYLINDRICAL_SURFACE ( 'NONE', #6009, 1.000000000000000888 ) ;
#4387 = VERTEX_POINT ( 'NONE', #4215 ) ;
#4388 = CIRCLE ( 'NONE', #14066, 12.49999999999999645 ) ;
#4389 = CARTESIAN_POINT ( 'NONE',  ( -2.712762565639006418, 3.052587955997511759, -3.430618716626627318 ) ) ;
#4390 = EDGE_CURVE ( 'NONE', #7769, #1337, #10793, .T. ) ;
#4391 = CARTESIAN_POINT ( 'NONE',  ( 45.90387839640214196, 58.69948385550240033, 5.676469297603166098 ) ) ;
#4392 = ADVANCED_FACE ( 'NONE', ( #5786 ), #5990, .F. ) ;
#4393 = DIRECTION ( 'NONE',  ( -0.000000000000000000, 0.000000000000000000, -1.000000000000000000 ) ) ;
#4394 = CARTESIAN_POINT ( 'NONE',  ( 56.66441430157294690, 46.90051614449765793, -2.141517661632166281 ) ) ;
#4395 = LINE ( 'NONE', #10361, #10447 ) ;
#4396 = CARTESIAN_POINT ( 'NONE',  ( 15.51323935927282704, -32.62297130559633729, 0.000000000000000000 ) ) ;
#4397 = AXIS2_PLACEMENT_3D ( 'NONE', #18806, #4085, #5643 ) ;
#4398 = CARTESIAN_POINT ( 'NONE',  ( -3.999999999998910649, -1.658469974638591804, -3.531532913075256186 ) ) ;
#4399 = ORIENTED_EDGE ( 'NONE', *, *, #2526, .F. ) ;
#4400 = ORIENTED_EDGE ( 'NONE', *, *, #8738, .F. ) ;
#4401 = ORIENTED_EDGE ( 'NONE', *, *, #1509, .F. ) ;
#4402 = CARTESIAN_POINT ( 'NONE',  ( -2.000000000000007550, -3.464101615137749945, 0.000000000000000000 ) ) ;
#4403 = AXIS2_PLACEMENT_3D ( 'NONE', #16645, #11917, #12014 ) ;
#4404 = CARTESIAN_POINT ( 'NONE',  ( 55.94051828345050836, 47.79948385550240886, -4.345558710429104465 ) ) ;
#4405 = LINE ( 'NONE', #13220, #15601 ) ;
#4406 = CIRCLE ( 'NONE', #1275, 1.000000000000000222 ) ;
#4407 = EDGE_LOOP ( 'NONE', ( #18429, #15682, #2350, #14629 ) ) ;
#4408 = CARTESIAN_POINT ( 'NONE',  ( -16.32050807568872841, -30.00000000000008171, 9.000000000000000000 ) ) ;
#4409 = AXIS2_PLACEMENT_3D ( 'NONE', #5912, #10413, #17692 ) ;
#4410 = ORIENTED_EDGE ( 'NONE', *, *, #11713, .T. ) ;
#4411 = CARTESIAN_POINT ( 'NONE',  ( 47.70284917648459810, 51.60051614449765367, 6.992620115222797139 ) ) ;
#4412 = ORIENTED_EDGE ( 'NONE', *, *, #1317, .T. ) ;
#4413 = EDGE_CURVE ( 'NONE', #4549, #17921, #16444, .T. ) ;
#4414 = UNCERTAINTY_MEASURE_WITH_UNIT (LENGTH_MEASURE( 1.000000000000000082E-05 ), #11985, 'distance_accuracy_value', 'NONE');
#4415 = CARTESIAN_POINT ( 'NONE',  ( 3.878096787214416530, -2.680238624820946214, 2.357690525401583415 ) ) ;
#4416 = ADVANCED_FACE ( 'NONE', ( #6082 ), #3148, .T. ) ;
#4418 = CONICAL_SURFACE ( 'NONE', #16317, 1.999999999999998224, 1.029744259999999745 ) ;
#4417 = CARTESIAN_POINT ( 'NONE',  ( 50.02271294988506156, 46.50051614449766646, -6.000000000000000888 ) ) ;
#4419 = CARTESIAN_POINT ( 'NONE',  ( 0.000000000000000000, -4.330127018922193649, -2.500000000000000000 ) ) ;
#4420 = EDGE_CURVE ( 'NONE', #12017, #2993, #14861, .T. ) ;
#4421 = DIRECTION ( 'NONE',  ( 0.000000000000000000, 0.000000000000000000, 1.000000000000000000 ) ) ;
#4422 = CARTESIAN_POINT ( 'NONE',  ( 44.91013252490152752, 56.79948385550240175, 3.727524721679198461 ) ) ;
#4423 = LINE ( 'NONE', #18155, #6931 ) ;
#4424 = AXIS2_PLACEMENT_3D ( 'NONE', #17611, #18791, #11209 ) ;
#4425 = CARTESIAN_POINT ( 'NONE',  ( 54.09612160359786515, 53.69948385550240744, -5.676469297603166098 ) ) ;
#4426 = AXIS2_PLACEMENT_3D ( 'NONE', #17204, #1023, #9728 ) ;
#4427 = CARTESIAN_POINT ( 'NONE',  ( 57.61547081786810764, 56.90051614449767214, -2.450534656007114176 ) ) ;
#4428 = DIRECTION ( 'NONE',  ( 0.000000000000000000, 0.000000000000000000, -1.000000000000000000 ) ) ;
#4429 = CARTESIAN_POINT ( 'NONE',  ( -150.9999999999999716, -14.99999999999999645, 15.00000000000000000 ) ) ;
#4430 = VERTEX_POINT ( 'NONE', #10283 ) ;
#4431 = DIRECTION ( 'NONE',  ( -0.000000000000000000, -0.000000000000000000, -1.000000000000000000 ) ) ;
#4432 = SURFACE_STYLE_USAGE ( .BOTH. , #17970 ) ;
#4433 = DIRECTION ( 'NONE',  ( -0.9999670257950101782, -0.008120795692649437902, -2.775557561562891351E-17 ) ) ;
#4434 = ORIENTED_EDGE ( 'NONE', *, *, #575, .F. ) ;
#4435 = FACE_BOUND ( 'NONE', #6746, .T. ) ;
#4436 = EDGE_CURVE ( 'NONE', #13007, #17145, #16274, .T. ) ;
#4437 = FACE_OUTER_BOUND ( 'NONE', #17799, .T. ) ;
#4438 = CIRCLE ( 'NONE', #16334, 2.649999999999985700 ) ;
#4439 = VECTOR ( 'NONE', #7550, 1000.000000000000000 ) ;
#4440 = ADVANCED_FACE ( 'NONE', ( #19342, #1575 ), #5884, .T. ) ;
#4441 = CARTESIAN_POINT ( 'NONE',  ( 16.79901371501572882, -9.146745271453649906, -9.000000000000000000 ) ) ;
#4442 = AXIS2_PLACEMENT_3D ( 'NONE', #12076, #9035, #6018 ) ;
#4443 = DIRECTION ( 'NONE',  ( -0.000000000000000000, -0.000000000000000000, -1.000000000000000000 ) ) ;
#4444 = FACE_OUTER_BOUND ( 'NONE', #4704, .T. ) ;
#4445 = CARTESIAN_POINT ( 'NONE',  ( -1.000000000000000222, -4.808326913195983821, -0.8000000000000000444 ) ) ;
#4446 = CARTESIAN_POINT ( 'NONE',  ( 50.02271294988512551, 60.49948385550240459, 7.000000000000000888 ) ) ;
#4447 = DIRECTION ( 'NONE',  ( 0.000000000000000000, 0.000000000000000000, 1.000000000000000000 ) ) ;
#4448 = CARTESIAN_POINT ( 'NONE',  ( 54.68390685589033495, 55.69948385550240744, -6.485486291978119766 ) ) ;
#4449 = DIRECTION ( 'NONE',  ( 0.000000000000000000, 0.000000000000000000, -1.000000000000000000 ) ) ;
#4450 = CARTESIAN_POINT ( 'NONE',  ( 47.70284917648459100, 57.60051614449764656, 6.992620115222796251 ) ) ;
#4451 = B_SPLINE_CURVE_WITH_KNOTS ( 'NONE', 3,
 ( #13690, #6247, #11032, #14068, #3406, #16943, #6345, #459, #6432, #12411, #267, #10841, #12224, #18233, #12317, #655 ),
 .UNSPECIFIED., .F., .F.,
 ( 4, 3, 3, 3, 3, 4 ),
 ( -2.669610558405663348E-06, 0.000000000000000000, 5.703179328867284594E-05, 0.0001157653700806020010, 0.0001686517580799737359, 0.0002219032271235107196 ),
 .UNSPECIFIED. ) ;
#4452 = DIRECTION ( 'NONE',  ( 1.000000000000000000, 0.000000000000000000, 0.000000000000000000 ) ) ;
#4453 = PRODUCT ( 'angular contact ball bearing_68_iso_ISO 15 ABB - 178 - 20,SI,NC,20_68', 'angular contact ball bearing_68_iso_ISO 15 ABB - 178 - 20,SI,NC,20_68', '', ( #5794 ) ) ;
#4454 = ORIENTED_EDGE ( 'NONE', *, *, #10466, .T. ) ;
#4455 = ORIENTED_EDGE ( 'NONE', *, *, #14348, .F. ) ;
#4456 = ORIENTED_EDGE ( 'NONE', *, *, #16591, .F. ) ;
#4457 = DIRECTION ( 'NONE',  ( 0.000000000000000000, 0.000000000000000000, -1.000000000000000000 ) ) ;
#4458 = ORIENTED_EDGE ( 'NONE', *, *, #9368, .T. ) ;
#4459 = CARTESIAN_POINT ( 'NONE',  ( 6.367873360227556567, 2.886751345948123770, -5.000000000000000000 ) ) ;
#4460 = ORIENTED_EDGE ( 'NONE', *, *, #5778, .F. ) ;
#4461 = FACE_OUTER_BOUND ( 'NONE', #4299, .T. ) ;
#4462 = VERTEX_POINT ( 'NONE', #10477 ) ;
#4463 = DIRECTION ( 'NONE',  ( -0.000000000000000000, -0.000000000000000000, 1.000000000000000000 ) ) ;
#4464 = CARTESIAN_POINT ( 'NONE',  ( 4.000000000000000000, 3.500000000000000000, 0.000000000000000000 ) ) ;
#4465 = CARTESIAN_POINT ( 'NONE',  ( 46.45491332379572924, 59.29948385550240886, -4.840751629271157874 ) ) ;
#4466 = CARTESIAN_POINT ( 'NONE',  ( -154.9999999999999716, -14.99999999999999645, 15.00000000000000000 ) ) ;
#4467 = DIRECTION ( 'NONE',  ( 0.000000000000000000, 0.000000000000000000, -1.000000000000000000 ) ) ;
#4468 = CARTESIAN_POINT ( 'NONE',  ( 47.42335538002180328, 54.40051614449765793, -8.007379884777206414 ) ) ;
#4469 = CARTESIAN_POINT ( 'NONE',  ( 56.30877334542961421, 51.00051614449765935, 0.02388180880515774693 ) ) ;
#4470 = CARTESIAN_POINT ( 'NONE',  ( 4.050536630291693641, -3.778525289263164222, -0.5912575323401421112 ) ) ;
#4471 = CARTESIAN_POINT ( 'NONE',  ( -154.9999999999999716, -14.99999999999999645, 15.79999999999999893 ) ) ;
#4472 = ORIENTED_EDGE ( 'NONE', *, *, #12996, .F. ) ;
#4473 = VECTOR ( 'NONE', #14745, 1000.000000000000000 ) ;
#4474 = ORIENTED_EDGE ( 'NONE', *, *, #13822, .T. ) ;
#4475 = DIRECTION ( 'NONE',  ( 0.000000000000000000, 0.000000000000000000, 1.000000000000000000 ) ) ;
#4476 = ORIENTED_EDGE ( 'NONE', *, *, #7820, .F. ) ;
#4477 = EDGE_CURVE ( 'NONE', #10516, #7873, #13293, .T. ) ;
#4478 = CARTESIAN_POINT ( 'NONE',  ( 57.36023556966787851, 61.99948385550241170, -0.02388180880522424582 ) ) ;
#4479 =( LENGTH_UNIT ( ) NAMED_UNIT ( * ) SI_UNIT ( .MILLI., .METRE. ) );
#4480 = CARTESIAN_POINT ( 'NONE',  ( -1.828356344711647319, -3.563200125723192002, -1.076197711133951296E-14 ) ) ;
#4481 = ORIENTED_EDGE ( 'NONE', *, *, #14777, .F. ) ;
#4482 = CARTESIAN_POINT ( 'NONE',  ( 53.50000000000000000, 0.000000000000000000, 0.000000000000000000 ) ) ;
#4483 = PRODUCT_RELATED_PRODUCT_CATEGORY ( 'part', '', ( #15860 ) ) ;
#4484 = CARTESIAN_POINT ( 'NONE',  ( 44.05948171654949874, 48.79948385550239465, 4.345558710429104465 ) ) ;
#4485 = EDGE_CURVE ( 'NONE', #16860, #728, #6109, .T. ) ;
#4486 = ORIENTED_EDGE ( 'NONE', *, *, #13455, .T. ) ;
#4487 = CARTESIAN_POINT ( 'NONE',  ( 2.649999999999988365, 15.00000000000001599, 15.00000000000000000 ) ) ;
#4488 = ORIENTED_EDGE ( 'NONE', *, *, #6281, .F. ) ;
#4489 = CARTESIAN_POINT ( 'NONE',  ( 54.68390685589033495, 49.69948385550240744, -6.485486291978119766 ) ) ;
#4490 = CARTESIAN_POINT ( 'NONE',  ( 49.99999999999997158, 45.00000000000001421, -6.500000000000004441 ) ) ;
#4491 = ADVANCED_FACE ( 'NONE', ( #16866 ), #3430, .F. ) ;
#4492 = EDGE_CURVE ( 'NONE', #17668, #7530, #1793, .T. ) ;
#4493 = CARTESIAN_POINT ( 'NONE',  ( 50.02271294988512551, 60.49948385550240459, 7.000000000000000888 ) ) ;
#4494 = DIRECTION ( 'NONE',  ( 0.000000000000000000, 0.000000000000000000, 1.000000000000000000 ) ) ;
#4495 = CARTESIAN_POINT ( 'NONE',  ( -129.9999999999999716, -14.99999999999999645, -3.999999999999999112 ) ) ;
#4496 = CARTESIAN_POINT ( 'NONE',  ( 56.66441430157294690, 52.90051614449765793, -2.141517661632166281 ) ) ;
#4497 = DIRECTION ( 'NONE',  ( 0.000000000000000000, 0.000000000000000000, -1.000000000000000000 ) ) ;
#4498 = EDGE_CURVE ( 'NONE', #6955, #1750, #18651, .T. ) ;
#4499 = FILL_AREA_STYLE ('',( #8988 ) ) ;
#4500 = CARTESIAN_POINT ( 'NONE',  ( 11.75570504584926468, -3.819660112500910198, -9.000000000000000000 ) ) ;
#4501 = ORIENTED_EDGE ( 'NONE', *, *, #2957, .F. ) ;
#4502 = ORIENTED_EDGE ( 'NONE', *, *, #18699, .T. ) ;
#4503 = ORIENTED_EDGE ( 'NONE', *, *, #184, .T. ) ;
#4504 = CARTESIAN_POINT ( 'NONE',  ( -1.312671235360383548, -3.860931062424228788, -0.05923475698271369466 ) ) ;
#4505 = ADVANCED_FACE ( 'NONE', ( #1865, #10859 ), #13894, .T. ) ;
#4506 = CARTESIAN_POINT ( 'NONE',  ( 43.18075615816989199, 63.19948385550240744, -4.924951120819313743 ) ) ;
#4507 = EDGE_CURVE ( 'NONE', #1247, #17702, #3613, .T. ) ;
#4508 = DIRECTION ( 'NONE',  ( -0.000000000000000000, -0.000000000000000000, 1.000000000000000000 ) ) ;
#4509 = ORIENTED_EDGE ( 'NONE', *, *, #17943, .T. ) ;
#4510 = CARTESIAN_POINT ( 'NONE',  ( 6.495567275915080430, 5.834887664329775347, 9.410860448829699171E-16 ) ) ;
#4511 = ORIENTED_EDGE ( 'NONE', *, *, #2696, .T. ) ;
#4512 = CARTESIAN_POINT ( 'NONE',  ( 45.86712807150329496, 61.70051614449766220, 5.649768623646139964 ) ) ;
#4513 = VERTEX_POINT ( 'NONE', #6449 ) ;
#4514 = CARTESIAN_POINT ( 'NONE',  ( 6.355827204229362870, -5.411702751981846582, 0.8440485055075620524 ) ) ;
#4515 = DIRECTION ( 'NONE',  ( -0.000000000000000000, 0.000000000000000000, 1.000000000000000000 ) ) ;
#4516 = CARTESIAN_POINT ( 'NONE',  ( 48.02776887271750184, 53.60051614449765367, 5.992620115222795363 ) ) ;
#4517 = CARTESIAN_POINT ( 'NONE',  ( 0.4465819873852049926, -5.773502691896263528, -3.127607256515468906E-17 ) ) ;
#4518 = CIRCLE ( 'NONE', #13881, 4.000000000000031086 ) ;
#4519 = LINE ( 'NONE', #13621, #17110 ) ;
#4520 = CARTESIAN_POINT ( 'NONE',  ( 44.30067958973596376, 56.89948385550240317, 1.875703265242204099 ) ) ;
#4521 = CARTESIAN_POINT ( 'NONE',  ( 4.236525694536557474, -2.416953475386482530, -3.751298745799839462 ) ) ;
#4522 = CARTESIAN_POINT ( 'NONE',  ( 52.29715082351547295, 52.39948385550241738, 6.992620115222774047 ) ) ;
#4523 = AXIS2_PLACEMENT_3D ( 'NONE', #13255, #9818, #8558 ) ;
#4524 = CARTESIAN_POINT ( 'NONE',  ( 41.58830220609386430, 56.00051614449765935, -0.02388180880514929535 ) ) ;
#4525 = CARTESIAN_POINT ( 'NONE',  ( 6.207530437345012864, -4.849805425595699937, 1.599890596045217439 ) ) ;
#4526 = CARTESIAN_POINT ( 'NONE',  ( 3.878096787214415642, 2.680238624820947990, -2.357690525401575421 ) ) ;
#4527 = ORIENTED_EDGE ( 'NONE', *, *, #5708, .F. ) ;
#4528 = DIRECTION ( 'NONE',  ( -1.000000000000000000, 0.000000000000000000, 0.000000000000000000 ) ) ;
#4529 = SURFACE_STYLE_FILL_AREA ( #16096 ) ;
#4530 = EDGE_LOOP ( 'NONE', ( #7481, #5283, #8817, #3012 ) ) ;
#4531 = LINE ( 'NONE', #7461, #3933 ) ;
#4532 = AXIS2_PLACEMENT_3D ( 'NONE', #15814, #6878, #17392 ) ;
#4533 = CARTESIAN_POINT ( 'NONE',  ( -20.63749999999999929, 5.633375276077824112E-16, 4.599999999999999645 ) ) ;
#4534 = AXIS2_PLACEMENT_3D ( 'NONE', #2173, #15305, #18460 ) ;
#4535 = CARTESIAN_POINT ( 'NONE',  ( 56.65037692655918988, 63.89948385550239607, -2.184720259617163762 ) ) ;
#4536 = CARTESIAN_POINT ( 'NONE',  ( 6.403457969954081008, 2.888443235695449030, 5.002930439003169028 ) ) ;
#4537 = CARTESIAN_POINT ( 'NONE',  ( 6.196878017913830305, -1.924500897298744961, 4.999999999999999112 ) ) ;
#4538 = CARTESIAN_POINT ( 'NONE',  ( -4.000000000000000000, -2.309401076758515803, -0.4999999999999995559 ) ) ;
#4539 = CARTESIAN_POINT ( 'NONE',  ( 52.25172492374522903, 55.59948385550241312, -7.007379884777225953 ) ) ;
#4540 = CARTESIAN_POINT ( 'NONE',  ( 50.00000000000000000, 40.00000000000000000, 0.000000000000000000 ) ) ;
#4541 = CARTESIAN_POINT ( 'NONE',  ( 50.02271294988513972, 52.49948385550241170, 8.000000000000001776 ) ) ;
#4542 = CARTESIAN_POINT ( 'NONE',  ( -10.93224627749309796, -3.252283996668732691, -9.000000000000000000 ) ) ;
#4543 = CARTESIAN_POINT ( 'NONE',  ( 52.25172492374527877, 55.40051614449764372, 7.007379884777203749 ) ) ;
#4544 = EDGE_CURVE ( 'NONE', #4327, #12719, #5797, .T. ) ;
#4545 = DIRECTION ( 'NONE',  ( -0.000000000000000000, -0.000000000000000000, 1.000000000000000000 ) ) ;
#4546 = AXIS2_PLACEMENT_3D ( 'NONE', #13714, #11052, #479 ) ;
#4547 = ORIENTED_EDGE ( 'NONE', *, *, #5091, .T. ) ;
#4548 = EDGE_CURVE ( 'NONE', #1857, #19012, #16768, .T. ) ;
#4549 = VERTEX_POINT ( 'NONE', #9201 ) ;
#4550 = AXIS2_PLACEMENT_3D ( 'NONE', #18472, #249, #12663 ) ;
#4551 = CARTESIAN_POINT ( 'NONE',  ( 18.00000000000000355, -20.00000000000000000, -12.00000000000000000 ) ) ;
#4552 = ORIENTED_EDGE ( 'NONE', *, *, #4590, .F. ) ;
#4553 = CARTESIAN_POINT ( 'NONE',  ( -54.99999999999996447, -6.999999999999985789, 15.00000000000000000 ) ) ;
#4554 = CARTESIAN_POINT ( 'NONE',  ( 56.66441430157296821, 62.09948385550239891, 2.141517661632100111 ) ) ;
#4555 = ORIENTED_EDGE ( 'NONE', *, *, #2825, .T. ) ;
#4556 = AXIS2_PLACEMENT_3D ( 'NONE', #10834, #6145, #9183 ) ;
#4557 = DIRECTION ( 'NONE',  ( 1.000000000000000000, 0.000000000000000000, 0.000000000000000000 ) ) ;
#4558 = ORIENTED_EDGE ( 'NONE', *, *, #10222, .T. ) ;
#4559 = CARTESIAN_POINT ( 'NONE',  ( 5.000000000000003553, -20.00000000000000000, -20.00000000000000000 ) ) ;
#4560 = FACE_OUTER_BOUND ( 'NONE', #18353, .T. ) ;
#4561 = CARTESIAN_POINT ( 'NONE',  ( 55.71335778527780747, 54.09948385550241312, 1.832500667257165983 ) ) ;
#4562 = DIRECTION ( 'NONE',  ( 0.000000000000000000, 0.000000000000000000, -1.000000000000000000 ) ) ;
#4563 = DIRECTION ( 'NONE',  ( -0.000000000000000000, -0.000000000000000000, 1.000000000000000000 ) ) ;
#4564 = CARTESIAN_POINT ( 'NONE',  ( 50.02271294988505446, 56.50051614449767357, -8.000000000000001776 ) ) ;
#4565 = AXIS2_PLACEMENT_3D ( 'NONE', #2367, #5098, #9690 ) ;
#4566 = CARTESIAN_POINT ( 'NONE',  ( 53.54508667620424234, 52.70051614449766220, -4.840751629271188961 ) ) ;
#4567 = CARTESIAN_POINT ( 'NONE',  ( -179.9999999999999716, -14.99999999999999289, 3.999999999999999112 ) ) ;
#4568 = FACE_OUTER_BOUND ( 'NONE', #16154, .T. ) ;
#4569 = ORIENTED_EDGE ( 'NONE', *, *, #1377, .F. ) ;
#4570 = AXIS2_PLACEMENT_3D ( 'NONE', #17353, #5276, #15676 ) ;
#4571 = ORIENTED_EDGE ( 'NONE', *, *, #8039, .F. ) ;
#4572 = CARTESIAN_POINT ( 'NONE',  ( 6.506892073925696351, 2.992473431090949543, -5.000000000000000000 ) ) ;
#4573 = EDGE_LOOP ( 'NONE', ( #14130, #9789 ) ) ;
#4574 = CARTESIAN_POINT ( 'NONE',  ( 49.97728705011488159, 65.49948385550240459, -7.000000000000000888 ) ) ;
#4575 = CARTESIAN_POINT ( 'NONE',  ( 0.1717365941144614327, -6.008326913195983998, -0.8000000000000000444 ) ) ;
#4576 = EDGE_LOOP ( 'NONE', ( #9252, #17651 ) ) ;
#4577 = CYLINDRICAL_SURFACE ( 'NONE', #3156, 2.000000000000001776 ) ;
#4578 = AXIS2_PLACEMENT_3D ( 'NONE', #188, #12135, #1367 ) ;
#4579 = CARTESIAN_POINT ( 'NONE',  ( 54.13287192849676188, 48.29948385550240175, 5.649768623646098220 ) ) ;
#4580 = ORIENTED_EDGE ( 'NONE', *, *, #5083, .T. ) ;
#4581 = DIRECTION ( 'NONE',  ( 0.000000000000000000, 0.000000000000000000, -1.000000000000000000 ) ) ;
#4582 = ORIENTED_EDGE ( 'NONE', *, *, #7956, .F. ) ;
#4583 = CARTESIAN_POINT ( 'NONE',  ( 52.62207051974829852, 62.60051614449765367, -7.992620115222797139 ) ) ;
#4584 = CARTESIAN_POINT ( 'NONE',  ( 52.60990417590917900, 44.99999999999999289, -5.983956152663589378 ) ) ;
#4585 = CARTESIAN_POINT ( 'NONE',  ( 43.33558569842703179, 61.09948385550240602, -2.141517661632099223 ) ) ;
#4586 = CARTESIAN_POINT ( 'NONE',  ( -5.130877905917297532, -0.6693483836015048372, -9.000000000000000000 ) ) ;
#4587 = VECTOR ( 'NONE', #16481, 1000.000000000000000 ) ;
#4588 = CARTESIAN_POINT ( 'NONE',  ( 54.09612160359792199, 55.30051614449765651, 5.676469297603124353 ) ) ;
#4589 = CARTESIAN_POINT ( 'NONE',  ( -20.00000000000000000, -25.00000000000000000, -20.00000000000000000 ) ) ;
#4590 = EDGE_CURVE ( 'NONE', #3807, #15831, #18329, .T. ) ;
#4591 = PRESENTATION_STYLE_ASSIGNMENT (( #8893 ) ) ;
#4592 = CARTESIAN_POINT ( 'NONE',  ( -4.000000000000000000, -1.680117682357936904, -3.316611593218794951 ) ) ;
#4593 = ORIENTED_EDGE ( 'NONE', *, *, #4350, .F. ) ;
#4594 = EDGE_LOOP ( 'NONE', ( #3777, #5571, #17551 ) ) ;
#4595 = ORIENTED_EDGE ( 'NONE', *, *, #10584, .T. ) ;
#4596 = CARTESIAN_POINT ( 'NONE',  ( 3.951447005078450925, 3.704664227300100254, -0.5833333333333329263 ) ) ;
#4597 = CARTESIAN_POINT ( 'NONE',  ( 42.39856655714566358, 62.89948385550240317, 2.493737253992119207 ) ) ;
#4598 = FACE_OUTER_BOUND ( 'NONE', #13539, .T. ) ;
#4599 = ORIENTED_EDGE ( 'NONE', *, *, #11189, .T. ) ;
#4600 = CARTESIAN_POINT ( 'NONE',  ( 73.00000000000002842, -1.000000000000000000, 6.000000000000001776 ) ) ;
#4601 = EDGE_CURVE ( 'NONE', #5231, #13890, #4896, .T. ) ;
#4602 = ORIENTED_EDGE ( 'NONE', *, *, #17189, .T. ) ;
#4603 = CARTESIAN_POINT ( 'NONE',  ( 44.05948171654945611, 62.20051614449765509, -4.345558710429044069 ) ) ;
#4604 = VERTEX_POINT ( 'NONE', #7923 ) ;
#4605 = VECTOR ( 'NONE', #4463, 1000.000000000000000 ) ;
#4606 = DIRECTION ( 'NONE',  ( 0.3420201433256622736, 0.000000000000000000, -0.9396926207859106484 ) ) ;
#4607 = UNCERTAINTY_MEASURE_WITH_UNIT (LENGTH_MEASURE( 1.000000000000000082E-05 ), #13095, 'distance_accuracy_value', 'NONE');
#4608 = CARTESIAN_POINT ( 'NONE',  ( -59.84999999999998721, 32.50000000000001421, -15.00000000000000000 ) ) ;
#4609 = CARTESIAN_POINT ( 'NONE',  ( 44.28664221472221385, 53.90051614449765793, 1.832500667257213722 ) ) ;
#4610 = DIRECTION ( 'NONE',  ( 1.000000000000000000, 0.000000000000000000, 0.000000000000000000 ) ) ;
#4611 = ADVANCED_FACE ( 'NONE', ( #18437, #10959 ), #2150, .F. ) ;
#4612 = VECTOR ( 'NONE', #4443, 1000.000000000000000 ) ;
#4613 = LINE ( 'NONE', #13324, #19332 ) ;
#4614 = ADVANCED_FACE ( 'NONE', ( #9294 ), #3521, .F. ) ;
#4615 = CARTESIAN_POINT ( 'NONE',  ( 53.50833635130540955, 55.69948385550240744, -4.867452303228209765 ) ) ;
#4616 = DIRECTION ( 'NONE',  ( 0.000000000000000000, 0.000000000000000000, 1.000000000000000000 ) ) ;
#4617 = CARTESIAN_POINT ( 'NONE',  ( 45.31609314410960820, 52.30051614449766362, -6.485486291978072693 ) ) ;
#4618 = CARTESIAN_POINT ( 'NONE',  ( 6.541334219041335274, -2.934241909852036478, 5.143243597038029691 ) ) ;
#4619 = AXIS2_PLACEMENT_3D ( 'NONE', #3092, #15039, #10322 ) ;
#4620 = DIRECTION ( 'NONE',  ( 0.000000000000000000, 0.000000000000000000, 1.000000000000000000 ) ) ;
#4621 = ORIENTED_EDGE ( 'NONE', *, *, #651, .F. ) ;
#4622 = CARTESIAN_POINT ( 'NONE',  ( 0.000000000000000000, -4.330127018922193649, -2.500000000000000000 ) ) ;
#4623 = PRESENTATION_STYLE_ASSIGNMENT (( #18355 ) ) ;
#4624 = AXIS2_PLACEMENT_3D ( 'NONE', #7543, #6080, #16675 ) ;
#4625 = EDGE_CURVE ( 'NONE', #15442, #4903, #13987, .T. ) ;
#4626 = ITEM_DEFINED_TRANSFORMATION ( 'NONE', 'NONE', #3433,  #10359 ) ;
#4627 = VERTEX_POINT ( 'NONE', #197 ) ;
#4628 = DIRECTION ( 'NONE',  ( 1.000000000000000000, 0.000000000000000000, -0.000000000000000000 ) ) ;
#4629 = DIRECTION ( 'NONE',  ( 0.02857142857142857401, 0.9995917534020515305, -0.000000000000000000 ) ) ;
#4630 = CIRCLE ( 'NONE', #7753, 7.000000000000000000 ) ;
#4631 = VECTOR ( 'NONE', #1305, 999.9999999999998863 ) ;
#4632 = CARTESIAN_POINT ( 'NONE',  ( 52.29715082351547295, 62.39948385550240317, 6.992620115222774047 ) ) ;
#4633 = CYLINDRICAL_SURFACE ( 'NONE', #16829, 5.999999999999977796 ) ;
#4634 = CIRCLE ( 'NONE', #7132, 2.500000000000000444 ) ;
#4635 = FACE_OUTER_BOUND ( 'NONE', #19090, .T. ) ;
#4636 = CARTESIAN_POINT ( 'NONE',  ( -22.14999999999999858, -19.99999999999999289, -23.00000000000000000 ) ) ;
#4637 = ADVANCED_FACE ( 'NONE', ( #4711 ), #18543, .F. ) ;
#4638 = CARTESIAN_POINT ( 'NONE',  ( 57.36023556966787851, 59.99948385550240459, -0.02388180880522424582 ) ) ;
#4639 = DIRECTION ( 'NONE',  ( -0.000000000000000000, 0.000000000000000000, -1.000000000000000000 ) ) ;
#4640 = CARTESIAN_POINT ( 'NONE',  ( 52.62207051974839089, 56.39948385550241028, 7.992620115222770494 ) ) ;
#4641 = LINE ( 'NONE', #11876, #15387 ) ;
#4642 = CARTESIAN_POINT ( 'NONE',  ( 43.34962307344078880, 54.10051614449766788, -2.184720259617096705 ) ) ;
#4643 = VECTOR ( 'NONE', #5032, 1000.000000000000000 ) ;
#4644 = FACE_OUTER_BOUND ( 'NONE', #10586, .T. ) ;
#4645 = ORIENTED_EDGE ( 'NONE', *, *, #19255, .F. ) ;
#4646 = AXIS2_PLACEMENT_3D ( 'NONE', #13540, #4431, #4528 ) ;
#4647 = VERTEX_POINT ( 'NONE', #1765 ) ;
#4648 = CARTESIAN_POINT ( 'NONE',  ( 6.534224484704323821, 2.950930484791612685, -5.111161529262899350 ) ) ;
#4649 = ORIENTED_EDGE ( 'NONE', *, *, #14215, .F. ) ;
#4650 = CARTESIAN_POINT ( 'NONE',  ( 6.196878017913831194, 3.367876570272813730, -4.166666666666668739 ) ) ;
#4651 = EDGE_CURVE ( 'NONE', #514, #11891, #18924, .T. ) ;
#4652 = DIRECTION ( 'NONE',  ( -0.000000000000000000, 0.000000000000000000, 1.000000000000000000 ) ) ;
#4653 = CARTESIAN_POINT ( 'NONE',  ( 0.3208286057739604957, -4.433571671609698228, -0.3503314178412692548 ) ) ;
#4654 = ORIENTED_EDGE ( 'NONE', *, *, #18569, .T. ) ;
#4655 = DIRECTION ( 'NONE',  ( 0.000000000000000000, 0.000000000000000000, 1.000000000000000000 ) ) ;
#4656 = VECTOR ( 'NONE', #4508, 1000.000000000000000 ) ;
#4657 = DIRECTION ( 'NONE',  ( 1.000000000000000000, 0.000000000000000000, 0.000000000000000000 ) ) ;
#4658 = ADVANCED_FACE ( 'NONE', ( #2556 ), #11537, .T. ) ;
#4659 = CIRCLE ( 'NONE', #12459, 4.000000000000003553 ) ;
#4660 = CARTESIAN_POINT ( 'NONE',  ( 56.30877334542961421, 55.99948385550241170, -0.02388180880520959434 ) ) ;
#4661 = DIRECTION ( 'NONE',  ( 0.000000000000000000, 0.000000000000000000, 1.000000000000000000 ) ) ;
#4662 = FACE_BOUND ( 'NONE', #6040, .T. ) ;
#4663 = CARTESIAN_POINT ( 'NONE',  ( 54.72065718078918906, 50.70051614449766220, -6.458785618021089192 ) ) ;
#4664 = CARTESIAN_POINT ( 'NONE',  ( 56.30877334542961421, 53.00051614449765935, 0.02388180880515774693 ) ) ;
#4665 =( GEOMETRIC_REPRESENTATION_CONTEXT ( 3 ) GLOBAL_UNCERTAINTY_ASSIGNED_CONTEXT ( ( #13615 ) ) GLOBAL_UNIT_ASSIGNED_CONTEXT ( ( #10846, #12229, #10754 ) ) REPRESENTATION_CONTEXT ( 'NONE', 'WORKASPACE' ) );
#4666 = DIRECTION ( 'NONE',  ( -1.000000000000000000, 0.000000000000000000, 1.224646799147353207E-16 ) ) ;
#4667 = CARTESIAN_POINT ( 'NONE',  ( 7.500000000000003553, -20.00000000000000000, -10.00000000000000000 ) ) ;
#4668 = ORIENTED_EDGE ( 'NONE', *, *, #1847, .F. ) ;
#4669 = VERTEX_POINT ( 'NONE', #4005 ) ;
#4670 = CYLINDRICAL_SURFACE ( 'NONE', #8743, 1.000000000000000888 ) ;
#4671 = ORIENTED_EDGE ( 'NONE', *, *, #19370, .F. ) ;
#4672 = MECHANICAL_DESIGN_GEOMETRIC_PRESENTATION_REPRESENTATION (  '', ( #4964 ), #8404 ) ;
#4673 = AXIS2_PLACEMENT_3D ( 'NONE', #11228, #6632, #3800 ) ;
#4674 = DIRECTION ( 'NONE',  ( 0.000000000000000000, -0.000000000000000000, 1.000000000000000000 ) ) ;
#4675 = DIRECTION ( 'NONE',  ( 0.000000000000000000, -1.000000000000000000, 0.000000000000000000 ) ) ;
#4676 = SHAPE_REPRESENTATION ( 'idle roller', ( #10359 ), #12782 ) ;
#4677 = VERTEX_POINT ( 'NONE', #13017 ) ;
#4678 = CYLINDRICAL_SURFACE ( 'NONE', #12220, 1.000000000000000888 ) ;
#4679 = CARTESIAN_POINT ( 'NONE',  ( 44.05948171654949874, 46.79948385550240175, 4.345558710429104465 ) ) ;
#4680 = EDGE_CURVE ( 'NONE', #9490, #11811, #969, .T. ) ;
#4681 = ORIENTED_EDGE ( 'NONE', *, *, #9384, .F. ) ;
#4682 = AXIS2_PLACEMENT_3D ( 'NONE', #15603, #2183, #3742 ) ;
#4683 = DIRECTION ( 'NONE',  ( 1.000000000000000000, 0.000000000000000000, 0.000000000000000000 ) ) ;
#4684 = ORIENTED_EDGE ( 'NONE', *, *, #14182, .F. ) ;
#4685 = CARTESIAN_POINT ( 'NONE',  ( 56.79116909180255135, 47.79948385550240886, -4.963592699179005585 ) ) ;
#4686 = DIRECTION ( 'NONE',  ( 0.000000000000000000, 0.000000000000000000, -1.000000000000000000 ) ) ;
#4687 = CARTESIAN_POINT ( 'NONE',  ( 45.86712807150323812, 57.29948385550240175, -5.649768623646098220 ) ) ;
#4688 = DIRECTION ( 'NONE',  ( -0.000000000000000000, -0.000000000000000000, -1.000000000000000000 ) ) ;
#4689 =( NAMED_UNIT ( * ) SI_UNIT ( $, .STERADIAN. ) SOLID_ANGLE_UNIT ( ) );
#4690 = CARTESIAN_POINT ( 'NONE',  ( 57.36023556966787851, 55.00051614449765225, 0.02388180880515038476 ) ) ;
#4691 = LINE ( 'NONE', #11193, #1074 ) ;
#4692 = AXIS2_PLACEMENT_3D ( 'NONE', #5847, #70, #6046 ) ;
#4693 = DIRECTION ( 'NONE',  ( 0.000000000000000000, 0.000000000000000000, -1.000000000000000000 ) ) ;
#4694 = CARTESIAN_POINT ( 'NONE',  ( -1.566204647097437563, -6.822536405429463713, 0.000000000000000000 ) ) ;
#4695 = EDGE_LOOP ( 'NONE', ( #17550, #19003, #11844, #17218, #8897, #6661, #8715, #12787 ) ) ;
#4696 = CIRCLE ( 'NONE', #3146, 6.080745460913608902 ) ;
#4697 = EDGE_LOOP ( 'NONE', ( #1759, #17403, #16084, #19108, #3768, #7361, #14692, #7390, #12661, #11357, #8074, #8079, #15171, #17463, #15535, #12226, #4943, #4323, #15579, #12090, #11431, #12510, #17356, #4073, #11425 ) ) ;
#4698 = EDGE_LOOP ( 'NONE', ( #11796, #16545, #10726, #5768 ) ) ;
#4699 = DIRECTION ( 'NONE',  ( -0.9135454576426043083, 0.4067366430757925477, 0.000000000000000000 ) ) ;
#4700 = CARTESIAN_POINT ( 'NONE',  ( 54.68390685589033495, 63.69948385550240033, -6.485486291978119766 ) ) ;
#4701 = VERTEX_POINT ( 'NONE', #17544 ) ;
#4702 = CARTESIAN_POINT ( 'NONE',  ( -4.000000000000000888, -2.309401076758512694, -3.504269196027526512 ) ) ;
#4703 = AXIS2_PLACEMENT_3D ( 'NONE', #16401, #14611, #4042 ) ;
#4704 = EDGE_LOOP ( 'NONE', ( #4813, #15884, #2162, #16622 ) ) ;
#4705 = CARTESIAN_POINT ( 'NONE',  ( 44.05948171654945611, 56.20051614449765509, -4.345558710429044069 ) ) ;
#4706 = ORIENTED_EDGE ( 'NONE', *, *, #10750, .F. ) ;
#4707 = CARTESIAN_POINT ( 'NONE',  ( 1.250000000000001110, 0.000000000000000000, -5.899999999999999467 ) ) ;
#4708 = CARTESIAN_POINT ( 'NONE',  ( -5.560781378645575757, 6.809993116116508640E-16, -4.000000000000000000 ) ) ;
#4709 = AXIS2_PLACEMENT_3D ( 'NONE', #12386, #437, #6406 ) ;
#4710 = CARTESIAN_POINT ( 'NONE',  ( 49.97728705011494554, 57.50051614449766646, 6.000000000000000888 ) ) ;
#4711 = FACE_OUTER_BOUND ( 'NONE', #9286, .T. ) ;
#4712 = CARTESIAN_POINT ( 'NONE',  ( 53.50833635130540955, 59.69948385550240744, -4.867452303228209765 ) ) ;
#4713 = DIRECTION ( 'NONE',  ( 0.000000000000000000, -0.4999999999999991118, 0.8660254037844391517 ) ) ;
#4714 = CARTESIAN_POINT ( 'NONE',  ( 57.61547081786810764, 54.90051614449765793, -2.450534656007114176 ) ) ;
#4715 = DIRECTION ( 'NONE',  ( 0.000000000000000000, -1.000000000000000000, 0.000000000000000000 ) ) ;
#4716 = AXIS2_PLACEMENT_3D ( 'NONE', #2558, #15677, #1163 ) ;
#4717 = VECTOR ( 'NONE', #1537, 1000.000000000000000 ) ;
#4718 = VERTEX_POINT ( 'NONE', #5273 ) ;
#4719 = CARTESIAN_POINT ( 'NONE',  ( -0.4472135954999577612, 0.000000000000000000, 0.000000000000000000 ) ) ;
#4720 = CARTESIAN_POINT ( 'NONE',  ( 2.000000000000000000, -0.8865213383406694847, 1.535500000000001419 ) ) ;
#4721 = VECTOR ( 'NONE', #8042, 1000.000000000000000 ) ;
#4722 = ORIENTED_EDGE ( 'NONE', *, *, #4865, .F. ) ;
#4723 = DIRECTION ( 'NONE',  ( 0.000000000000000000, 0.000000000000000000, 1.000000000000000000 ) ) ;
#4724 = ADVANCED_FACE ( 'NONE', ( #4105 ), #864, .T. ) ;
#4725 = CARTESIAN_POINT ( 'NONE',  ( 4.175813232069148562, 4.122719923832741884, -2.765695189283172261E-17 ) ) ;
#4726 = TOROIDAL_SURFACE ( 'NONE', #15679, 5.200000000000001066, 0.4999999999999978351 ) ;
#4727 = EDGE_CURVE ( 'NONE', #17826, #8815, #2980, .T. ) ;
#4728 = CARTESIAN_POINT ( 'NONE',  ( 42.63976443033212149, 60.99948385550239749, 0.02388180880522514787 ) ) ;
#4729 = AXIS2_PLACEMENT_3D ( 'NONE', #8218, #770, #3818 ) ;
#4730 = DIRECTION ( 'NONE',  ( 0.000000000000000000, 1.000000000000000000, -1.224646799147353207E-16 ) ) ;
#4731 = CIRCLE ( 'NONE', #6913, 20.00000000000000000 ) ;
#4732 = DIRECTION ( 'NONE',  ( 2.191393683118470056E-17, 7.538405132783724027E-17, 1.000000000000000000 ) ) ;
#4733 = EDGE_CURVE ( 'NONE', #7722, #4891, #18958, .T. ) ;
#4734 = EDGE_CURVE ( 'NONE', #6996, #18140, #12051, .T. ) ;
#4735 = DIRECTION ( 'NONE',  ( 0.000000000000000000, 0.000000000000000000, -1.000000000000000000 ) ) ;
#4736 = CARTESIAN_POINT ( 'NONE',  ( 42.63976443033212860, 58.99948385550239038, 0.02388180880522514787 ) ) ;
#4737 = AXIS2_PLACEMENT_3D ( 'NONE', #327, #16997, #10889 ) ;
#4738 = CARTESIAN_POINT ( 'NONE',  ( -159.0000000000000000, -14.99999999999999645, -17.00000000000000000 ) ) ;
#4739 = CARTESIAN_POINT ( 'NONE',  ( 45.31609314410967926, 54.69948385550240033, 6.485486291978119766 ) ) ;
#4740 = PLANE ( 'NONE',  #3501 ) ;
#4741 = CARTESIAN_POINT ( 'NONE',  ( 47.70284917648459100, 55.60051614449764656, 6.992620115222796251 ) ) ;
#4742 = ADVANCED_FACE ( 'NONE', ( #11245 ), #15968, .F. ) ;
#4743 = CARTESIAN_POINT ( 'NONE',  ( -4.197393957002303999, -7.773935952363655451E-14, -3.503767560748929810 ) ) ;
#4744 = VECTOR ( 'NONE', #9385, 1000.000000000000000 ) ;
#4745 = SURFACE_STYLE_USAGE ( .BOTH. , #16998 ) ;
#4746 = AXIS2_PLACEMENT_3D ( 'NONE', #11340, #14766, #9959 ) ;
#4747 = VERTEX_POINT ( 'NONE', #10072 ) ;
#4748 = EDGE_CURVE ( 'NONE', #2946, #11693, #9675, .T. ) ;
#4749 = EDGE_CURVE ( 'NONE', #18696, #18359, #18831, .T. ) ;
#4750 = CARTESIAN_POINT ( 'NONE',  ( -1.250000000000001110, 0.000000000000000000, 0.000000000000000000 ) ) ;
#4751 = CARTESIAN_POINT ( 'NONE',  ( 49.97728705011495265, 49.50051614449765935, 7.000000000000000888 ) ) ;
#4752 = DIRECTION ( 'NONE',  ( 1.000000000000000000, 0.000000000000000000, 0.000000000000000000 ) ) ;
#4753 = LINE ( 'NONE', #1621, #18397 ) ;
#4754 = EDGE_LOOP ( 'NONE', ( #15836, #9958, #6897, #17122, #11407, #9667, #563, #15561 ) ) ;
#4755 = DIRECTION ( 'NONE',  ( 0.000000000000000000, 0.000000000000000000, -1.000000000000000000 ) ) ;
#4756 = CARTESIAN_POINT ( 'NONE',  ( -74.99999999999997158, -1.000000000000000000, 6.000000000000001776 ) ) ;
#4757 = CARTESIAN_POINT ( 'NONE',  ( 55.71335778527780036, 44.90051614449765793, -1.832500667257213056 ) ) ;
#4758 = DIRECTION ( 'NONE',  ( -1.000000000000000000, -0.000000000000000000, -0.000000000000000000 ) ) ;
#4759 = FACE_OUTER_BOUND ( 'NONE', #18, .T. ) ;
#4760 = AXIS2_PLACEMENT_3D ( 'NONE', #11167, #2281, #16993 ) ;
#4761 = CARTESIAN_POINT ( 'NONE',  ( 45.27934281921082516, 53.70051614449766220, 6.458785618021089192 ) ) ;
#4762 = CARTESIAN_POINT ( 'NONE',  ( 46.49166364869456913, 54.30051614449765651, -4.867452303228181343 ) ) ;
#4763 = VECTOR ( 'NONE', #17399, 1000.000000000000000 ) ;
#4764 = CARTESIAN_POINT ( 'NONE',  ( -4.197393957002303999, -7.773935952363655451E-14, -3.503767560748929810 ) ) ;
#4765 = CARTESIAN_POINT ( 'NONE',  ( 0.000000000000000000, 0.000000000000000000, -9.000000000000001776 ) ) ;
#4766 = VERTEX_POINT ( 'NONE', #1064 ) ;
#4767 = VERTEX_POINT ( 'NONE', #6650 ) ;
#4768 = CARTESIAN_POINT ( 'NONE',  ( 6.212060063025226064, 2.039954613758735658, -5.000000000000000000 ) ) ;
#4769 = VERTEX_POINT ( 'NONE', #12921 ) ;
#4770 = LINE ( 'NONE', #535, #12181 ) ;
#4771 = ORIENTED_EDGE ( 'NONE', *, *, #12858, .F. ) ;
#4772 = DIRECTION ( 'NONE',  ( -0.000000000000000000, -0.000000000000000000, -1.000000000000000000 ) ) ;
#4773 = CARTESIAN_POINT ( 'NONE',  ( 42.63976443033212149, 52.99948385550240459, 0.02388180880522514787 ) ) ;
#4774 = ORIENTED_EDGE ( 'NONE', *, *, #19004, .T. ) ;
#4775 = CARTESIAN_POINT ( 'NONE',  ( 0.8816464618332836567, -24.71833652004169934, 9.000000000000000000 ) ) ;
#4776 = EDGE_LOOP ( 'NONE', ( #6330, #9142, #709, #16239 ) ) ;
#4777 = CARTESIAN_POINT ( 'NONE',  ( 42.38452918213190657, 63.90051614449765793, 2.450534656007115508 ) ) ;
#4778 = CYLINDRICAL_SURFACE ( 'NONE', #12324, 1.000000000000000000 ) ;
#4779 = CARTESIAN_POINT ( 'NONE',  ( 43.33558569842703179, 57.09948385550240602, -2.141517661632099223 ) ) ;
#4780 = CARTESIAN_POINT ( 'NONE',  ( 0.9999999999999997780, -6.008326913195983998, -0.8000000000000000444 ) ) ;
#4781 = FILL_AREA_STYLE_COLOUR ( '', #19049 ) ;
#4782 = CARTESIAN_POINT ( 'NONE',  ( 49.97728705011495265, 53.50051614449765935, 7.000000000000000888 ) ) ;
#4783 = DIRECTION ( 'NONE',  ( 1.000000000000000000, 0.000000000000000000, 0.000000000000000000 ) ) ;
#4784 = AXIS2_PLACEMENT_3D ( 'NONE', #8985, #7802, #371 ) ;
#4785 = B_SPLINE_CURVE_WITH_KNOTS ( 'NONE', 3,
 ( #17486, #19263, #17772, #1200, #19169, #7072, #10110, #4045 ),
 .UNSPECIFIED., .F., .F.,
 ( 4, 2, 2, 4 ),
 ( 1.228285202167177233E-19, 0.001493104274552340370, 0.002986208549104680306, 0.005972417098209360613 ),
 .UNSPECIFIED. ) ;
#4786 = DIRECTION ( 'NONE',  ( 1.000000000000000000, 0.000000000000000000, 0.000000000000000000 ) ) ;
#4787 = EDGE_LOOP ( 'NONE', ( #8005, #10366, #16026, #5421 ) ) ;
#4788 = EDGE_CURVE ( 'NONE', #15338, #5469, #7034, .T. ) ;
#4789 = ORIENTED_EDGE ( 'NONE', *, *, #6763, .F. ) ;
#4790 = VERTEX_POINT ( 'NONE', #18631 ) ;
#4791 = FACE_OUTER_BOUND ( 'NONE', #639, .T. ) ;
#4792 = SURFACE_STYLE_FILL_AREA ( #16665 ) ;
#4793 = ADVANCED_FACE ( 'NONE', ( #11346 ), #5172, .F. ) ;
#4794 = CARTESIAN_POINT ( 'NONE',  ( 44.05948171654949874, 54.79948385550241596, 4.345558710429105354 ) ) ;
#4795 = FACE_OUTER_BOUND ( 'NONE', #17846, .T. ) ;
#4796 = VERTEX_POINT ( 'NONE', #15674 ) ;
#4797 = DIRECTION ( 'NONE',  ( 0.000000000000000000, 0.000000000000000000, 1.000000000000000000 ) ) ;
#4798 = EDGE_LOOP ( 'NONE', ( #13012, #17902, #9560, #10457 ) ) ;
#4799 = CARTESIAN_POINT ( 'NONE',  ( 52.29715082351539479, 58.60051614449766078, -6.992620115222796251 ) ) ;
#4800 = VERTEX_POINT ( 'NONE', #8217 ) ;
#4801 = DIRECTION ( 'NONE',  ( 0.000000000000000000, 0.000000000000000000, 1.000000000000000000 ) ) ;
#4802 = UNCERTAINTY_MEASURE_WITH_UNIT (LENGTH_MEASURE( 1.000000000000000082E-05 ), #11254, 'distance_accuracy_value', 'NONE');
#4803 = DIRECTION ( 'NONE',  ( 1.000000000000000000, 0.000000000000000000, 0.000000000000000000 ) ) ;
#4804 = PRODUCT_DEFINITION_FORMATION_WITH_SPECIFIED_SOURCE ( 'ANY', '', #11148, .NOT_KNOWN. ) ;
#4805 = CARTESIAN_POINT ( 'NONE',  ( 55.69932041026405045, 53.10051614449767499, 1.875703265242156359 ) ) ;
#4806 = DIRECTION ( 'NONE',  ( 0.000000000000000000, -1.000000000000000000, -0.000000000000000000 ) ) ;
#4807 = CARTESIAN_POINT ( 'NONE',  ( 0.000000000000000000, 0.000000000000000000, 5.000000000000000000 ) ) ;
#4808 = CARTESIAN_POINT ( 'NONE',  ( 44.91013252490152752, 64.79948385550240175, 3.727524721679198461 ) ) ;
#4809 = DIRECTION ( 'NONE',  ( 1.000000000000000000, 0.000000000000000000, -0.000000000000000000 ) ) ;
#4810 = CARTESIAN_POINT ( 'NONE',  ( 50.02271294988505446, 56.50051614449767357, -8.000000000000001776 ) ) ;
#4811 = ORIENTED_EDGE ( 'NONE', *, *, #18171, .F. ) ;
#4812 = FACE_OUTER_BOUND ( 'NONE', #6564, .T. ) ;
#4813 = ORIENTED_EDGE ( 'NONE', *, *, #15484, .F. ) ;
#4814 = FACE_OUTER_BOUND ( 'NONE', #10938, .T. ) ;
#4815 = ITEM_DEFINED_TRANSFORMATION ( 'NONE', 'NONE', #918,  #10359 ) ;
#4816 = ORIENTED_EDGE ( 'NONE', *, *, #3307, .T. ) ;
#4817 = FACE_OUTER_BOUND ( 'NONE', #12300, .T. ) ;
#4818 = LINE ( 'NONE', #10781, #610 ) ;
#4819 = CYLINDRICAL_SURFACE ( 'NONE', #7205, 2.649999999999985700 ) ;
#4820 = CARTESIAN_POINT ( 'NONE',  ( 3.951447005078450925, 2.357513599190970144, 2.916666666666667407 ) ) ;
#4821 = VECTOR ( 'NONE', #4639, 1000.000000000000000 ) ;
#4822 = CYLINDRICAL_SURFACE ( 'NONE', #4833, 2.649999999999985700 ) ;
#4823 = CARTESIAN_POINT ( 'NONE',  ( -17.79870116617242459, -29.12174527145394265, -9.000000000000000000 ) ) ;
#4824 = CARTESIAN_POINT ( 'NONE',  ( 54.09612160359786515, 55.69948385550240744, -5.676469297603166098 ) ) ;
#4825 = CYLINDRICAL_SURFACE ( 'NONE', #17287, 6.080745460913608902 ) ;
#4826 = CARTESIAN_POINT ( 'NONE',  ( 52.57664461997811856, 61.59948385550240602, -8.007379884777229506 ) ) ;
#4827 = EDGE_CURVE ( 'NONE', #17914, #8147, #9227, .T. ) ;
#4828 = CARTESIAN_POINT ( 'NONE',  ( 50.02271294988505446, 56.50051614449766646, -7.000000000000000888 ) ) ;
#4829 = CARTESIAN_POINT ( 'NONE',  ( 0.4465819873852002742, 2.886751345948125547, 4.999999999999999112 ) ) ;
#4830 = CARTESIAN_POINT ( 'NONE',  ( 53.50000000000000000, 0.000000000000000000, 3.309499999999999886 ) ) ;
#4831 = VECTOR ( 'NONE', #14029, 1000.000000000000000 ) ;
#4832 = ORIENTED_EDGE ( 'NONE', *, *, #15508, .F. ) ;
#4833 = AXIS2_PLACEMENT_3D ( 'NONE', #10983, #16990, #15491 ) ;
#4834 = CARTESIAN_POINT ( 'NONE',  ( 15.00000000000000178, -20.00000000000000000, -23.00000000000000000 ) ) ;
#4835 = CARTESIAN_POINT ( 'NONE',  ( 56.66441430157294690, 46.90051614449765793, -2.141517661632166281 ) ) ;
#4836 = EDGE_CURVE ( 'NONE', #12060, #13420, #17254, .T. ) ;
#4837 = CARTESIAN_POINT ( 'NONE',  ( 10.93224627749321876, -36.74771600333119181, -9.000000000000000000 ) ) ;
#4838 = EDGE_CURVE ( 'NONE', #3598, #16920, #2449, .T. ) ;
#4839 = DIRECTION ( 'NONE',  ( 0.000000000000000000, 0.000000000000000000, 1.000000000000000000 ) ) ;
#4840 = ORIENTED_EDGE ( 'NONE', *, *, #14283, .T. ) ;
#4841 = FACE_OUTER_BOUND ( 'NONE', #11042, .T. ) ;
#4842 = PLANE ( 'NONE',  #15789 ) ;
#4843 = CARTESIAN_POINT ( 'NONE',  ( 51.92680522751238925, 45.40051614449765793, 6.007379884777208190 ) ) ;
#4844 = CARTESIAN_POINT ( 'NONE',  ( 4.154306624731035846, -2.398490048085128556, -3.721999068284417955 ) ) ;
#4845 = DIRECTION ( 'NONE',  ( -0.000000000000000000, 0.000000000000000000, -1.000000000000000000 ) ) ;
#4846 = CARTESIAN_POINT ( 'NONE',  ( 54.68390685589039890, 61.30051614449766362, 6.485486291978072693 ) ) ;
#4847 = AXIS2_PLACEMENT_3D ( 'NONE', #1961, #10674, #12430 ) ;
#4848 = EDGE_CURVE ( 'NONE', #9274, #6054, #13309, .T. ) ;
#4849 = CARTESIAN_POINT ( 'NONE',  ( 44.30067958973594955, 56.10051614449766078, -1.875703265242155693 ) ) ;
#4850 = ADVANCED_FACE ( 'NONE', ( #10259 ), #8604, .T. ) ;
#4851 = CARTESIAN_POINT ( 'NONE',  ( 62.49999999999998579, 45.00000000000001421, -15.00000000000000000 ) ) ;
#4852 = DIRECTION ( 'NONE',  ( -0.000000000000000000, -0.000000000000000000, 1.000000000000000000 ) ) ;
#4853=STYLED_ITEM('',(#19475),#8977);
#4854 = ORIENTED_EDGE ( 'NONE', *, *, #11794, .F. ) ;
#4855 = VERTEX_POINT ( 'NONE', #7234 ) ;
#4856 = CARTESIAN_POINT ( 'NONE',  ( 6.507056081706568129, -2.993351035583803110, -4.999999999999999112 ) ) ;
#4857 = VERTEX_POINT ( 'NONE', #5964 ) ;
#4858 = EDGE_CURVE ( 'NONE', #2243, #10511, #2496, .T. ) ;
#4859 = PLANE ( 'NONE',  #3440 ) ;
#4860 = ADVANCED_FACE ( 'NONE', ( #4292 ), #16363, .F. ) ;
#4861 = ORIENTED_EDGE ( 'NONE', *, *, #16482, .F. ) ;
#4862 = CIRCLE ( 'NONE', #3928, 0.9999999999999995559 ) ;
#4863 = CARTESIAN_POINT ( 'NONE',  ( 2.449293598294706513E-15, -20.00000000000000000, -8.999999999999998224 ) ) ;
#4864 = CARTESIAN_POINT ( 'NONE',  ( 47.74827507625477807, 54.59948385550239891, 7.007379884777229506 ) ) ;
#4865 = EDGE_CURVE ( 'NONE', #8472, #7823, #18028, .T. ) ;
#4866 = VERTEX_POINT ( 'NONE', #8801 ) ;
#4867 = DIRECTION ( 'NONE',  ( 0.000000000000000000, 0.000000000000000000, 1.000000000000000000 ) ) ;
#4868 = EDGE_LOOP ( 'NONE', ( #12573, #13501, #16712, #6610 ) ) ;
#4869 = CARTESIAN_POINT ( 'NONE',  ( 42.38452918213188525, 47.09948385550240602, -2.450534656007040013 ) ) ;
#4870 = DIRECTION ( 'NONE',  ( 0.000000000000000000, -0.000000000000000000, 1.000000000000000000 ) ) ;
#4871 = VECTOR ( 'NONE', #10193, 1000.000000000000000 ) ;
#4872 = CARTESIAN_POINT ( 'NONE',  ( 44.30067958973596376, 46.89948385550240317, 1.875703265242204099 ) ) ;
#4873 = CARTESIAN_POINT ( 'NONE',  ( -44.99999999999997158, -40.00000000000000000, -10.00000000000000000 ) ) ;
#4874 = CARTESIAN_POINT ( 'NONE',  ( -154.9999999999999716, -14.99999999999999645, 6.499999999999999112 ) ) ;
#4875 = CARTESIAN_POINT ( 'NONE',  ( 47.70284917648459100, 61.60051614449764656, 6.992620115222796251 ) ) ;
#4876 = CARTESIAN_POINT ( 'NONE',  ( 0.000000000000000000, 0.000000000000000000, -1.000000000000000000 ) ) ;
#4877 = CARTESIAN_POINT ( 'NONE',  ( 42.63976443033212860, 52.99948385550240459, 0.02388180880522514787 ) ) ;
#4878 = DIRECTION ( 'NONE',  ( 0.000000000000000000, 1.000000000000000000, -9.783878858594328898E-16 ) ) ;
#4879 = APPLICATION_CONTEXT ( 'automotive_design' ) ;
#4880 = EDGE_LOOP ( 'NONE', ( #12199, #3184 ) ) ;
#4881 = EDGE_LOOP ( 'NONE', ( #3226, #5476, #14041, #10011 ) ) ;
#4882 = DIRECTION ( 'NONE',  ( 0.000000000000000000, 0.000000000000000000, 1.000000000000000000 ) ) ;
#4883 = VECTOR ( 'NONE', #14788, 999.9999999999998863 ) ;
#4884 = CARTESIAN_POINT ( 'NONE',  ( 52.25172492374522903, 49.59948385550240602, -7.007379884777225953 ) ) ;
#4885 =( NAMED_UNIT ( * ) SI_UNIT ( $, .STERADIAN. ) SOLID_ANGLE_UNIT ( ) );
#4886 = ORIENTED_EDGE ( 'NONE', *, *, #14851, .F. ) ;
#4887 = CARTESIAN_POINT ( 'NONE',  ( -72.99999999999997158, 2.999999999999999112, -20.00000000000000000 ) ) ;
#4888 = VECTOR ( 'NONE', #4898, 1000.000000000000000 ) ;
#4889 = ORIENTED_EDGE ( 'NONE', *, *, #13719, .T. ) ;
#4890 = CARTESIAN_POINT ( 'NONE',  ( 3.799999999999999378, 0.000000000000000000, -0.8000000000000000444 ) ) ;
#4891 = VERTEX_POINT ( 'NONE', #13115 ) ;
#4892 = EDGE_CURVE ( 'NONE', #19035, #16243, #8891, .T. ) ;
#4893 = PLANE ( 'NONE',  #15064 ) ;
#4894 = FACE_OUTER_BOUND ( 'NONE', #7689, .T. ) ;
#4895 = CARTESIAN_POINT ( 'NONE',  ( 53.50833635130544508, 53.30051614449767072, 4.867452303228181343 ) ) ;
#4896 = LINE ( 'NONE', #12144, #1407 ) ;
#4897 = EDGE_CURVE ( 'NONE', #6925, #18236, #19123, .T. ) ;
#4898 = DIRECTION ( 'NONE',  ( -1.000000000000000000, 9.251858538542972814E-17, -0.000000000000000000 ) ) ;
#4899 = DIRECTION ( 'NONE',  ( -0.000000000000000000, 0.000000000000000000, -1.000000000000000000 ) ) ;
#4900 = CARTESIAN_POINT ( 'NONE',  ( 57.61547081786810764, 60.90051614449766504, -2.450534656007114176 ) ) ;
#4901 = VERTEX_POINT ( 'NONE', #14576 ) ;
#4902 = DIRECTION ( 'NONE',  ( 0.000000000000000000, 0.000000000000000000, -1.000000000000000000 ) ) ;
#4903 = VERTEX_POINT ( 'NONE', #4589 ) ;
#4904 = LINE ( 'NONE', #10871, #13097 ) ;
#4905 = ORIENTED_EDGE ( 'NONE', *, *, #13922, .T. ) ;
#4906 = AXIS2_PLACEMENT_3D ( 'NONE', #1421, #7585, #10517 ) ;
#4907 = DIRECTION ( 'NONE',  ( 1.000000000000000000, 0.000000000000000000, 0.000000000000000000 ) ) ;
#4908 = CARTESIAN_POINT ( 'NONE',  ( 2.649999999999988365, 15.00000000000001599, 15.00000000000000000 ) ) ;
#4909 = CARTESIAN_POINT ( 'NONE',  ( 0.1713913650100259145, 0.000000000000000000, 0.000000000000000000 ) ) ;
#4910 = CARTESIAN_POINT ( 'NONE',  ( 0.000000000000000000, 0.000000000000000000, 0.000000000000000000 ) ) ;
#4911 = PLANE ( 'NONE',  #10154 ) ;
#4912 = AXIS2_PLACEMENT_3D ( 'NONE', #9524, #2191, #336 ) ;
#4913 = CARTESIAN_POINT ( 'NONE',  ( -2.804994570502171047, -3.229033611042465335, -3.526374918436838701 ) ) ;
#4914 = CARTESIAN_POINT ( 'NONE',  ( 56.65037692655918988, 63.89948385550239607, -2.184720259617163762 ) ) ;
#4915 = CARTESIAN_POINT ( 'NONE',  ( 6.244889965166094292, 3.924082311521017274, 3.413878157001050795 ) ) ;
#4916 = CIRCLE ( 'NONE', #5230, 1.535500000000000087 ) ;
#4917 = CARTESIAN_POINT ( 'NONE',  ( 47.37792948025162332, 59.39948385550240317, -7.992620115222770494 ) ) ;
#4918 = CARTESIAN_POINT ( 'NONE',  ( 45.90387839640208512, 62.30051614449766362, -5.676469297603124353 ) ) ;
#4919 = FACE_OUTER_BOUND ( 'NONE', #2408, .T. ) ;
#4920 = CYLINDRICAL_SURFACE ( 'NONE', #16636, 2.649999999999985700 ) ;
#4921 =( NAMED_UNIT ( * ) PLANE_ANGLE_UNIT ( ) SI_UNIT ( $, .RADIAN. ) );
#4922 = EDGE_LOOP ( 'NONE', ( #6440, #10323, #19281, #18216, #15107 ) ) ;
#4923 = AXIS2_PLACEMENT_3D ( 'NONE', #6950, #2362, #17456 ) ;
#4924 = CARTESIAN_POINT ( 'NONE',  ( -1.000000000000000222, -4.808326913195983821, 0.000000000000000000 ) ) ;
#4925 = CARTESIAN_POINT ( 'NONE',  ( 49.97728705011495265, 47.50051614449766646, 7.000000000000000888 ) ) ;
#4926 = CARTESIAN_POINT ( 'NONE',  ( 45.90387839640214196, 62.69948385550240744, 5.676469297603166098 ) ) ;
#4927 = CARTESIAN_POINT ( 'NONE',  ( -4.000000000000000000, 2.309401076758498483, -5.000000000000000000 ) ) ;
#4928 = VERTEX_POINT ( 'NONE', #11638 ) ;
#4929 = DIRECTION ( 'NONE',  ( 0.000000000000000000, 0.000000000000000000, -1.000000000000000000 ) ) ;
#4930 = CARTESIAN_POINT ( 'NONE',  ( 7.336184427528458230, 0.000000000000000000, 0.000000000000000000 ) ) ;
#4931 = CARTESIAN_POINT ( 'NONE',  ( 46.45491332379572924, 63.29948385550240175, -4.840751629271157874 ) ) ;
#4932 = CARTESIAN_POINT ( 'NONE',  ( -0.1717365941144614605, -6.008326913195983998, -0.8000000000000000444 ) ) ;
#4933 = CARTESIAN_POINT ( 'NONE',  ( -4.999999999999998224, -20.00000000000000000, -9.999999999999994671 ) ) ;
#4934 = AXIS2_PLACEMENT_3D ( 'NONE', #13039, #15892, #17277 ) ;
#4935 = CARTESIAN_POINT ( 'NONE',  ( 54.72065718078918906, 56.70051614449766930, -6.458785618021089192 ) ) ;
#4936 = CARTESIAN_POINT ( 'NONE',  ( 51.97223112728249816, 54.60051614449766788, -5.992620115222793586 ) ) ;
#4937 = VECTOR ( 'NONE', #10888, 1000.000000000000000 ) ;
#4938 = LINE ( 'NONE', #15335, #18840 ) ;
#4939 = DIRECTION ( 'NONE',  ( -0.000000000000000000, 1.000000000000000000, -0.000000000000000000 ) ) ;
#4940 = ORIENTED_EDGE ( 'NONE', *, *, #9990, .F. ) ;
#4941 = EDGE_LOOP ( 'NONE', ( #1584, #8466, #13261, #15641 ) ) ;
#4942 = CARTESIAN_POINT ( 'NONE',  ( 6.357965579934049316, -1.995168835099641713, -5.108766517442258959 ) ) ;
#4943 = ORIENTED_EDGE ( 'NONE', *, *, #4865, .T. ) ;
#4944 = DIRECTION ( 'NONE',  ( -1.000000000000000000, 0.000000000000000000, 0.000000000000000000 ) ) ;
#4945 = ORIENTED_EDGE ( 'NONE', *, *, #4350, .T. ) ;
#4946 = DIRECTION ( 'NONE',  ( -0.000000000000000000, -0.000000000000000000, 1.000000000000000000 ) ) ;
#4947 = EDGE_CURVE ( 'NONE', #14568, #2854, #4862, .T. ) ;
#4948 = CARTESIAN_POINT ( 'NONE',  ( 47.70284917648453415, 55.39948385550239607, -6.992620115222774047 ) ) ;
#4949 = VECTOR ( 'NONE', #8120, 1000.000000000000000 ) ;
#4950 = VERTEX_POINT ( 'NONE', #16457 ) ;
#4951 = CARTESIAN_POINT ( 'NONE',  ( 8.500000000000000000, 2.886751345948125991, 4.999999999999999112 ) ) ;
#4952 = VERTEX_POINT ( 'NONE', #19224 ) ;
#4953 = CARTESIAN_POINT ( 'NONE',  ( 57.61547081786812896, 56.09948385550240602, 2.450534656007040901 ) ) ;
#4954 = ADVANCED_FACE ( 'NONE', ( #10452 ), #1261, .T. ) ;
#4955 = CARTESIAN_POINT ( 'NONE',  ( 55.94051828345050836, 63.79948385550240886, -4.345558710429104465 ) ) ;
#4956 = CARTESIAN_POINT ( 'NONE',  ( 4.104070371397485317, 2.023683613428364225, -3.505122836902508698 ) ) ;
#4957 = CARTESIAN_POINT ( 'NONE',  ( 4.093692494532774617, -4.043567292011547742, 3.285329657490527105E-16 ) ) ;
#4958 = CARTESIAN_POINT ( 'NONE',  ( 49.97728705011495265, 59.50051614449765935, 7.000000000000000888 ) ) ;
#4959 = EDGE_CURVE ( 'NONE', #5570, #13074, #17398, .T. ) ;
#4960 = EDGE_CURVE ( 'NONE', #3410, #1462, #85, .T. ) ;
#4961 = CYLINDRICAL_SURFACE ( 'NONE', #6322, 4.000000000000000000 ) ;
#4962 = CARTESIAN_POINT ( 'NONE',  ( 55.96859303347804371, 60.19948385550240744, 4.306917132069425946 ) ) ;
#4963 = CARTESIAN_POINT ( 'NONE',  ( 19.30627432446651426, -25.22185519795840136, 0.000000000000000000 ) ) ;
#4964=STYLED_ITEM('',(#19482),#15206);
#4965 = ORIENTED_EDGE ( 'NONE', *, *, #16830, .F. ) ;
#4966 = CIRCLE ( 'NONE', #10293, 10.00000000000000888 ) ;
#4967 = EDGE_LOOP ( 'NONE', ( #8752, #4061, #10105, #4978 ) ) ;
#4968 = CARTESIAN_POINT ( 'NONE',  ( -3.309651814758565180, -5.455921364805393026, 0.000000000000000000 ) ) ;
#4969 = CARTESIAN_POINT ( 'NONE',  ( 43.33558569842703179, 51.09948385550240602, -2.141517661632099223 ) ) ;
#4970 = CARTESIAN_POINT ( 'NONE',  ( 0.4472135954999577612, 0.000000000000000000, 5.400000000000000355 ) ) ;
#4971 = STYLED_ITEM ( 'NONE', ( #4204 ), #7556 ) ;
#4972 = ORIENTED_EDGE ( 'NONE', *, *, #1133, .T. ) ;
#4973 = FACE_OUTER_BOUND ( 'NONE', #2732, .T. ) ;
#4974 = EDGE_CURVE ( 'NONE', #4179, #18236, #14773, .T. ) ;
#4975 = EDGE_CURVE ( 'NONE', #1337, #10178, #4205, .T. ) ;
#4976 = ORIENTED_EDGE ( 'NONE', *, *, #5015, .F. ) ;
#4977 = CARTESIAN_POINT ( 'NONE',  ( 49.97728705011495265, 63.50051614449765935, 7.000000000000000888 ) ) ;
#4978 = ORIENTED_EDGE ( 'NONE', *, *, #7115, .F. ) ;
#4979 = CIRCLE ( 'NONE', #18465, 1.000000000000000222 ) ;
#4980 = AXIS2_PLACEMENT_3D ( 'NONE', #11597, #1410, #8567 ) ;
#4981 = CARTESIAN_POINT ( 'NONE',  ( -18.02113032590308705, -13.81966011250110249, 9.000000000000000000 ) ) ;
#4982 = UNCERTAINTY_MEASURE_WITH_UNIT (LENGTH_MEASURE( 1.000000000000000082E-05 ), #9123, 'distance_accuracy_value', 'NONE');
#4983 = DIRECTION ( 'NONE',  ( 0.000000000000000000, 0.000000000000000000, 1.000000000000000000 ) ) ;
#4984 = CARTESIAN_POINT ( 'NONE',  ( 50.02271294988506156, 58.50051614449765225, -6.000000000000000888 ) ) ;
#4985 = DIRECTION ( 'NONE',  ( 0.000000000000000000, 0.000000000000000000, -1.000000000000000000 ) ) ;
#4986 = DIRECTION ( 'NONE',  ( -1.000000000000000000, 1.734723475976806848E-16, 0.000000000000000000 ) ) ;
#4987 = DIRECTION ( 'NONE',  ( 1.000000000000000000, 0.000000000000000000, 0.000000000000000000 ) ) ;
#4988 = CARTESIAN_POINT ( 'NONE',  ( 43.18075615816994173, 57.80051614449766362, 4.924951120819380357 ) ) ;
#4989 = ORIENTED_EDGE ( 'NONE', *, *, #5848, .F. ) ;
#4990 = ORIENTED_EDGE ( 'NONE', *, *, #11653, .T. ) ;
#4991 = DIRECTION ( 'NONE',  ( 0.000000000000000000, 0.000000000000000000, -1.000000000000000000 ) ) ;
#4992 = AXIS2_PLACEMENT_3D ( 'NONE', #12281, #18281, #1994 ) ;
#4993 = VECTOR ( 'NONE', #8123, 1000.000000000000000 ) ;
#4994 = SURFACE_SIDE_STYLE ('',( #12441 ) ) ;
#4995 = ORIENTED_EDGE ( 'NONE', *, *, #11347, .T. ) ;
#4996 = LINE ( 'NONE', #17461, #4246 ) ;
#4997 = DIRECTION ( 'NONE',  ( 0.000000000000000000, -0.8660254037844382635, -0.5000000000000008882 ) ) ;
#4998 = VECTOR ( 'NONE', #18868, 1000.000000000000000 ) ;
#5000 = EDGE_CURVE ( 'NONE', #15442, #189, #17049, .T. ) ;
#4999 = ORIENTED_EDGE ( 'NONE', *, *, #813, .T. ) ;
#5001 = EDGE_CURVE ( 'NONE', #8753, #5527, #4395, .T. ) ;
#5002 = CARTESIAN_POINT ( 'NONE',  ( 52.80949999999998568, 0.000000000000000000, 4.000000000000000000 ) ) ;
#5003 = UNCERTAINTY_MEASURE_WITH_UNIT (LENGTH_MEASURE( 1.000000000000000082E-05 ), #1553, 'distance_accuracy_value', 'NONE');
#5004 = CARTESIAN_POINT ( 'NONE',  ( 3.806834918298646731, 3.031088913245537864, 1.750000000000000666 ) ) ;
#5005 = AXIS2_PLACEMENT_3D ( 'NONE', #16542, #2921, #19413 ) ;
#5006 = DIRECTION ( 'NONE',  ( 1.000000000000000000, 0.000000000000000000, 0.000000000000000000 ) ) ;
#5007 = CARTESIAN_POINT ( 'NONE',  ( 4.747884751462026820, -5.143694235355983579, -0.8000000000000000444 ) ) ;
#5008 = CARTESIAN_POINT ( 'NONE',  ( 45.86712807150323812, 63.29948385550240886, -5.649768623646098220 ) ) ;
#5009 = DIRECTION ( 'NONE',  ( 1.000000000000000000, 0.000000000000000000, 0.000000000000000000 ) ) ;
#5010 = CARTESIAN_POINT ( 'NONE',  ( 52.57664461997811856, 59.59948385550240602, -8.007379884777229506 ) ) ;
#5011 = CARTESIAN_POINT ( 'NONE',  ( 54.09612160359792199, 59.30051614449766362, 5.676469297603124353 ) ) ;
#5012 = AXIS2_PLACEMENT_3D ( 'NONE', #9247, #2204, #13068 ) ;
#5013 = DIRECTION ( 'NONE',  ( -1.000000000000000000, 0.000000000000000000, 0.000000000000000000 ) ) ;
#5014 = DIRECTION ( 'NONE',  ( 0.000000000000000000, 0.000000000000000000, 1.000000000000000000 ) ) ;
#5015 = EDGE_CURVE ( 'NONE', #10511, #14216, #2930, .T. ) ;
#5016 = SHAPE_DEFINITION_REPRESENTATION ( #6762, #16703 ) ;
#5017 = VERTEX_POINT ( 'NONE', #18588 ) ;
#5018 = VECTOR ( 'NONE', #3066, 1000.000000000000000 ) ;
#5019 = CARTESIAN_POINT ( 'NONE',  ( -154.9999999999999716, -14.99999999999999645, 10.00000000000000000 ) ) ;
#5020 = EDGE_CURVE ( 'NONE', #8949, #17786, #4691, .T. ) ;
#5021 = LINE ( 'NONE', #13746, #13764 ) ;
#5022 = CIRCLE ( 'NONE', #6584, 0.9999999999999995559 ) ;
#5023 = AXIS2_PLACEMENT_3D ( 'NONE', #2018, #4946, #9352 ) ;
#5024 = CARTESIAN_POINT ( 'NONE',  ( 55.94051828345054389, 47.20051614449766220, 4.345558710429044957 ) ) ;
#5025 = LINE ( 'NONE', #18579, #12193 ) ;
#5026 = CIRCLE ( 'NONE', #17252, 1.999999999999998224 ) ;
#5027 = CARTESIAN_POINT ( 'NONE',  ( 8.134732861515777458, -1.729090847147875198, -9.000000000000000000 ) ) ;
#5028 = ORIENTED_EDGE ( 'NONE', *, *, #6748, .F. ) ;
#5029 = CARTESIAN_POINT ( 'NONE',  ( 2.482347295856823136E-15, -20.00000000000000000, -8.999999999999996447 ) ) ;
#5030 = CARTESIAN_POINT ( 'NONE',  ( 0.000000000000000000, 1.773042676681340524, -2.059984127722458425E-15 ) ) ;
#5031 = CARTESIAN_POINT ( 'NONE',  ( 46.49166364869460466, 62.69948385550240744, 4.867452303228209765 ) ) ;
#5032 = DIRECTION ( 'NONE',  ( 1.000000000000000000, 1.387778780781445676E-16, -0.000000000000000000 ) ) ;
#5033 = DIRECTION ( 'NONE',  ( -0.000000000000000000, -0.000000000000000000, -1.000000000000000000 ) ) ;
#5034 = DIRECTION ( 'NONE',  ( 0.000000000000000000, 0.000000000000000000, -1.000000000000000000 ) ) ;
#5035 = CARTESIAN_POINT ( 'NONE',  ( 43.20883090819742023, 62.20051614449766220, -4.963592699178938972 ) ) ;
#5036 = AXIS2_PLACEMENT_3D ( 'NONE', #9411, #12839, #3728 ) ;
#5037 = CARTESIAN_POINT ( 'NONE',  ( 49.97728705011494554, 61.50051614449766646, 6.000000000000000888 ) ) ;
#5038 = CARTESIAN_POINT ( 'NONE',  ( 2.000000000000000000, 0.000000000000000000, 0.000000000000000000 ) ) ;
#5039 = VECTOR ( 'NONE', #2255, 1000.000000000000000 ) ;
#5040 = DIRECTION ( 'NONE',  ( -0.9999670257950100671, -0.008120795692649436168, -2.775557561562891043E-17 ) ) ;
#5041 = VECTOR ( 'NONE', #12477, 999.9999999999998863 ) ;
#5042 = ORIENTED_EDGE ( 'NONE', *, *, #19370, .T. ) ;
#5043 = ORIENTED_EDGE ( 'NONE', *, *, #14825, .F. ) ;
#5044 = LINE ( 'NONE', #2894, #18163 ) ;
#5045 = ORIENTED_EDGE ( 'NONE', *, *, #15751, .T. ) ;
#5046 = CARTESIAN_POINT ( 'NONE',  ( -12.54977455159113653, -35.57251292194792569, 0.000000000000000000 ) ) ;
#5047 = ORIENTED_EDGE ( 'NONE', *, *, #17938, .T. ) ;
#5048 = DIRECTION ( 'NONE',  ( 0.000000000000000000, 0.000000000000000000, 1.000000000000000000 ) ) ;
#5049 = CARTESIAN_POINT ( 'NONE',  ( 45.86712807150323812, 53.29948385550240886, -5.649768623646098220 ) ) ;
#5050 = ORIENTED_EDGE ( 'NONE', *, *, #11929, .F. ) ;
#5051 = CARTESIAN_POINT ( 'NONE',  ( 1.599999999999999867, -5.408326913195983465, -0.8000000000000000444 ) ) ;
#5052 = VECTOR ( 'NONE', #7700, 1000.000000000000000 ) ;
#5053 = ORIENTED_EDGE ( 'NONE', *, *, #6989, .F. ) ;
#5054 = CARTESIAN_POINT ( 'NONE',  ( 42.38452918213188525, 51.09948385550240602, -2.450534656007040013 ) ) ;
#5055 = CARTESIAN_POINT ( 'NONE',  ( 4.033895293471413623, 1.419609371826631827, -3.500000000000000000 ) ) ;
#5056 = CARTESIAN_POINT ( 'NONE',  ( 43.33558569842703179, 63.09948385550240602, -2.141517661632099223 ) ) ;
#5057 = CARTESIAN_POINT ( 'NONE',  ( 3.878096787214571517, 3.381939201670116191, 1.142309474598433461 ) ) ;
#5058 = FACE_OUTER_BOUND ( 'NONE', #6710, .T. ) ;
#5059 = CARTESIAN_POINT ( 'NONE',  ( 45.86712807150329496, 59.70051614449766220, 5.649768623646139964 ) ) ;
#5060 = CARTESIAN_POINT ( 'NONE',  ( 44.05948171654949874, 56.79948385550240886, 4.345558710429105354 ) ) ;
#5061 = CARTESIAN_POINT ( 'NONE',  ( 0.6920835326022565237, 4.454600218803884459, -3.597382984111579862 ) ) ;
#5062 = CARTESIAN_POINT ( 'NONE',  ( 6.541171661047877173, -5.920857802016179505, -0.02973393389965061501 ) ) ;
#5063 = EDGE_CURVE ( 'NONE', #9040, #4202, #438, .T. ) ;
#5064 = ORIENTED_EDGE ( 'NONE', *, *, #8672, .T. ) ;
#5065 = ORIENTED_EDGE ( 'NONE', *, *, #2454, .F. ) ;
#5066 = DIRECTION ( 'NONE',  ( 1.000000000000000000, 0.000000000000000000, 0.000000000000000000 ) ) ;
#5067 = SURFACE_STYLE_FILL_AREA ( #17339 ) ;
#5068 = PRODUCT_RELATED_PRODUCT_CATEGORY ( 'part', '', ( #7416 ) ) ;
#5069 = CARTESIAN_POINT ( 'NONE',  ( 57.36023556966787851, 51.99948385550238328, -0.02388180880522424582 ) ) ;
#5070 = AXIS2_PLACEMENT_3D ( 'NONE', #7133, #12648, #16161 ) ;
#5071 = DIRECTION ( 'NONE',  ( -0.000000000000000000, 0.000000000000000000, 1.000000000000000000 ) ) ;
#5072 = VERTEX_POINT ( 'NONE', #9624 ) ;
#5073 = VERTEX_POINT ( 'NONE', #15721 ) ;
#5074 = CARTESIAN_POINT ( 'NONE',  ( -30.00000000000000000, -40.00000000000000711, 6.000000000000035527 ) ) ;
#5075 = EDGE_CURVE ( 'NONE', #488, #10416, #816, .T. ) ;
#5076 = EDGE_CURVE ( 'NONE', #16750, #3485, #5125, .T. ) ;
#5077 = VERTEX_POINT ( 'NONE', #520 ) ;
#5078 = CARTESIAN_POINT ( 'NONE',  ( 43.33558569842706021, 63.90051614449765793, 2.141517661632167169 ) ) ;
#5079 = ORIENTED_EDGE ( 'NONE', *, *, #15036, .T. ) ;
#5080 = EDGE_CURVE ( 'NONE', #7529, #2510, #758, .T. ) ;
#5081 = CARTESIAN_POINT ( 'NONE',  ( 55.94051828345050836, 47.79948385550240886, -4.345558710429104465 ) ) ;
#5082 = CARTESIAN_POINT ( 'NONE',  ( 12.54977455159103705, -4.427487078051979275, 0.000000000000000000 ) ) ;
#5083 = EDGE_CURVE ( 'NONE', #18931, #12414, #7324, .T. ) ;
#5084 = AXIS2_PLACEMENT_3D ( 'NONE', #14547, #7007, #12898 ) ;
#5085 = CARTESIAN_POINT ( 'NONE',  ( 55.69932041026405045, 59.10051614449766078, 1.875703265242156359 ) ) ;
#5086 = CARTESIAN_POINT ( 'NONE',  ( 2.385244779468109755E-15, -20.00000000000000000, -9.999999999999994671 ) ) ;
#5087 =( LENGTH_UNIT ( ) NAMED_UNIT ( * ) SI_UNIT ( .MILLI., .METRE. ) );
#5088 = CARTESIAN_POINT ( 'NONE',  ( -14.14213562373094568, -14.99999999999998757, -20.00000000000000000 ) ) ;
#5089 = ADVANCED_FACE ( 'NONE', ( #6691, #12773 ), #3476, .F. ) ;
#5090 = CARTESIAN_POINT ( 'NONE',  ( 57.60143344285435774, 57.10051614449766788, 2.493737253992045044 ) ) ;
#5091 = EDGE_CURVE ( 'NONE', #18115, #1014, #16980, .T. ) ;
#5092 = ORIENTED_EDGE ( 'NONE', *, *, #2928, .F. ) ;
#5093 = ORIENTED_EDGE ( 'NONE', *, *, #13389, .T. ) ;
#5094 = DIRECTION ( 'NONE',  ( -1.000000000000000000, 0.000000000000000000, 0.000000000000000000 ) ) ;
#5095 = DIRECTION ( 'NONE',  ( 0.000000000000000000, 0.000000000000000000, 1.000000000000000000 ) ) ;
#5096 = ITEM_DEFINED_TRANSFORMATION ( 'NONE', 'NONE', #18274,  #10359 ) ;
#5097 = ORIENTED_EDGE ( 'NONE', *, *, #17583, .F. ) ;
#5098 = DIRECTION ( 'NONE',  ( 0.000000000000000000, 0.000000000000000000, 1.000000000000000000 ) ) ;
#5099 = EDGE_CURVE ( 'NONE', #762, #6796, #3621, .T. ) ;
#5100 = CARTESIAN_POINT ( 'NONE',  ( -62.49999999999997158, 32.50000000000001421, -10.00000000000000178 ) ) ;
#5101 = EDGE_LOOP ( 'NONE', ( #17348, #1149, #5819, #12911 ) ) ;
#5102 = PRODUCT_DEFINITION_FORMATION_WITH_SPECIFIED_SOURCE ( 'ANY', '', #7416, .NOT_KNOWN. ) ;
#5103 = CARTESIAN_POINT ( 'NONE',  ( 8.500000000000000000, 0.000000000000000000, 0.000000000000000000 ) ) ;
#5104 = DIRECTION ( 'NONE',  ( 0.9999419836444144449, 0.01077169184824096695, 0.000000000000000000 ) ) ;
#5105 = CARTESIAN_POINT ( 'NONE',  ( -0.9996874511566050669, -39.97499999999999432, 0.000000000000000000 ) ) ;
#5106 = DIRECTION ( 'NONE',  ( 0.000000000000000000, 0.000000000000000000, 1.000000000000000000 ) ) ;
#5107 = CARTESIAN_POINT ( 'NONE',  ( 55.11794222512601493, 46.19948385550240744, 3.688883143319541702 ) ) ;
#5108 = DIRECTION ( 'NONE',  ( -1.000000000000000000, -0.000000000000000000, -0.000000000000000000 ) ) ;
#5109 = CARTESIAN_POINT ( 'NONE',  ( 56.81924384183011512, 58.19948385550240744, 4.924951120819313743 ) ) ;
#5110 = CARTESIAN_POINT ( 'NONE',  ( 55.94051828345053679, 63.20051614449765509, 4.345558710429044069 ) ) ;
#5111 = CARTESIAN_POINT ( 'NONE',  ( 5.130877905917027526, -0.6693483836014323396, -9.000000000000000000 ) ) ;
#5112 = DIRECTION ( 'NONE',  ( 1.000000000000000000, 0.000000000000000000, 0.000000000000000000 ) ) ;
#5113 = ORIENTED_EDGE ( 'NONE', *, *, #9863, .T. ) ;
#5114 = SURFACE_SIDE_STYLE ('',( #12857 ) ) ;
#5115 = CARTESIAN_POINT ( 'NONE',  ( -154.9999999999999716, -14.99999999999999645, 15.79999999999999893 ) ) ;
#5116 = CARTESIAN_POINT ( 'NONE',  ( 54.13287192849671214, 48.70051614449766220, -5.649768623646139964 ) ) ;
#5117 = CARTESIAN_POINT ( 'NONE',  ( 54.76112626223286384, 45.00000000000007816, -5.734953493745535091 ) ) ;
#5118 = LINE ( 'NONE', #17097, #17763 ) ;
#5119 = ORIENTED_EDGE ( 'NONE', *, *, #15675, .T. ) ;
#5120 = LINE ( 'NONE', #9434, #10842 ) ;
#5121 = CARTESIAN_POINT ( 'NONE',  ( 30.00000000000000000, -40.00000000000000711, 6.000000000000035527 ) ) ;
#5122 = EDGE_CURVE ( 'NONE', #10528, #7075, #13939, .T. ) ;
#5123 = CYLINDRICAL_SURFACE ( 'NONE', #15589, 8.000000000000007105 ) ;
#5124 = DIRECTION ( 'NONE',  ( -1.000000000000000000, -0.000000000000000000, -0.000000000000000000 ) ) ;
#5125 = LINE ( 'NONE', #3127, #3267 ) ;
#5126 = CARTESIAN_POINT ( 'NONE',  ( 57.60143344285435774, 61.10051614449766788, 2.493737253992045044 ) ) ;
#5127 = EDGE_CURVE ( 'NONE', #590, #8683, #9440, .T. ) ;
#5128 = CARTESIAN_POINT ( 'NONE',  ( 48.02776887271750184, 59.60051614449765367, 5.992620115222795363 ) ) ;
#5129 = AXIS2_PLACEMENT_3D ( 'NONE', #4262, #7200, #16228 ) ;
#5130 = CARTESIAN_POINT ( 'NONE',  ( 2.000000000000000000, -6.429618962271402616, -1.000000000000000000 ) ) ;
#5131 = CYLINDRICAL_SURFACE ( 'NONE', #13160, 2.649999999999988365 ) ;
#5132 = VECTOR ( 'NONE', #16698, 1000.000000000000000 ) ;
#5133 = ORIENTED_EDGE ( 'NONE', *, *, #2461, .F. ) ;
#5134 = ORIENTED_EDGE ( 'NONE', *, *, #17618, .T. ) ;
#5135 = DIRECTION ( 'NONE',  ( -1.387778780781445676E-16, 1.000000000000000000, 0.000000000000000000 ) ) ;
#5136 = ORIENTED_EDGE ( 'NONE', *, *, #13805, .T. ) ;
#5137 = CARTESIAN_POINT ( 'NONE',  ( -4.000000000000000000, 0.9868501483902560878, -0.09357334158579519445 ) ) ;
#5138 = ORIENTED_EDGE ( 'NONE', *, *, #5939, .T. ) ;
#5139 = DIRECTION ( 'NONE',  ( -1.000000000000000000, -0.000000000000000000, -0.000000000000000000 ) ) ;
#5140 = CARTESIAN_POINT ( 'NONE',  ( 54.13287192849676188, 50.29948385550240175, 5.649768623646098220 ) ) ;
#5141 = VERTEX_POINT ( 'NONE', #9086 ) ;
#5142 = FACE_OUTER_BOUND ( 'NONE', #4922, .T. ) ;
#5143 = VERTEX_POINT ( 'NONE', #5220 ) ;
#5144 = CARTESIAN_POINT ( 'NONE',  ( 50.02271294988513972, 52.49948385550241170, 8.000000000000001776 ) ) ;
#5145 = AXIS2_PLACEMENT_3D ( 'NONE', #17979, #27, #8742 ) ;
#5146 = DIRECTION ( 'NONE',  ( 0.000000000000000000, 0.000000000000000000, -1.000000000000000000 ) ) ;
#5147 = CARTESIAN_POINT ( 'NONE',  ( 43.34962307344081012, 64.89948385550239607, 2.184720259617164650 ) ) ;
#5148 = DIRECTION ( 'NONE',  ( 0.000000000000000000, -1.000000000000000000, 8.673617379884036458E-16 ) ) ;
#5149 = CARTESIAN_POINT ( 'NONE',  ( -6.259644161404860030E-16, -4.618802153517027165, -5.000000000000000000 ) ) ;
#5150 = CARTESIAN_POINT ( 'NONE',  ( 56.66441430157294690, 58.90051614449766504, -2.141517661632166281 ) ) ;
#5151 = CARTESIAN_POINT ( 'NONE',  ( 55.11794222512601493, 62.19948385550240744, 3.688883143319541702 ) ) ;
#5152 = CARTESIAN_POINT ( 'NONE',  ( 47.70284917648453415, 57.39948385550241028, -6.992620115222774047 ) ) ;
#5153 = CARTESIAN_POINT ( 'NONE',  ( 6.403457969954084561, -2.888443235695444145, 5.002930439003169028 ) ) ;
#5154 = CARTESIAN_POINT ( 'NONE',  ( 6.390820841722131718, -5.837016270311242039, -0.1100087447852515082 ) ) ;
#5155 = ORIENTED_EDGE ( 'NONE', *, *, #9324, .T. ) ;
#5156 = AXIS2_PLACEMENT_3D ( 'NONE', #10694, #12353, #11071 ) ;
#5157 = ORIENTED_EDGE ( 'NONE', *, *, #10236, .T. ) ;
#5158 = DIRECTION ( 'NONE',  ( 0.000000000000000000, 0.000000000000000000, 1.000000000000000000 ) ) ;
#5159 =( NAMED_UNIT ( * ) PLANE_ANGLE_UNIT ( ) SI_UNIT ( $, .RADIAN. ) );
#5160 = CARTESIAN_POINT ( 'NONE',  ( 55.96859303347804371, 52.19948385550240033, 4.306917132069425946 ) ) ;
#5161 = CARTESIAN_POINT ( 'NONE',  ( -18.89043790736547379, -17.90943073464699609, -9.000000000000000000 ) ) ;
#5162 = VERTEX_POINT ( 'NONE', #8255 ) ;
#5163 = ORIENTED_EDGE ( 'NONE', *, *, #18080, .T. ) ;
#5164 = DIRECTION ( 'NONE',  ( -0.000000000000000000, -0.000000000000000000, -1.000000000000000000 ) ) ;
#5165 = ORIENTED_EDGE ( 'NONE', *, *, #4413, .F. ) ;
#5166 = CARTESIAN_POINT ( 'NONE',  ( 20.00000000000000000, -25.00000000000000711, -23.00000000000000000 ) ) ;
#5167 = ORIENTED_EDGE ( 'NONE', *, *, #15756, .F. ) ;
#5168 = EDGE_CURVE ( 'NONE', #4549, #9525, #14205, .T. ) ;
#5169 = CARTESIAN_POINT ( 'NONE',  ( -9.999999999999994671, 20.00000000000001421, 15.00000000000000000 ) ) ;
#5170 = LINE ( 'NONE', #11142, #10219 ) ;
#5171 = CARTESIAN_POINT ( 'NONE',  ( 48.02776887271750184, 61.60051614449765367, 5.992620115222795363 ) ) ;
#5172 = CYLINDRICAL_SURFACE ( 'NONE', #788, 5.999999999999977796 ) ;
#5173 = DIRECTION ( 'NONE',  ( -0.000000000000000000, -0.000000000000000000, -1.000000000000000000 ) ) ;
#5174 = CARTESIAN_POINT ( 'NONE',  ( -11.75570504584948139, -3.819660112501066518, 9.000000000000000000 ) ) ;
#5175 = AXIS2_PLACEMENT_3D ( 'NONE', #15201, #13544, #1779 ) ;
#5176 = CARTESIAN_POINT ( 'NONE',  ( 49.97728705011495265, 57.50051614449766646, 8.000000000000001776 ) ) ;
#5177 = VERTEX_POINT ( 'NONE', #14135 ) ;
#5178 = ORIENTED_EDGE ( 'NONE', *, *, #7458, .F. ) ;
#5179 = DIRECTION ( 'NONE',  ( -0.000000000000000000, -0.000000000000000000, -1.000000000000000000 ) ) ;
#5180 = AXIS2_PLACEMENT_3D ( 'NONE', #12629, #17546, #18925 ) ;
#5181 = LINE ( 'NONE', #10970, #10933 ) ;
#5182 = ADVANCED_FACE ( 'NONE', ( #8058 ), #14231, .F. ) ;
#5183 = ORIENTED_EDGE ( 'NONE', *, *, #7411, .T. ) ;
#5184 = DIRECTION ( 'NONE',  ( -0.000000000000000000, -0.000000000000000000, -1.000000000000000000 ) ) ;
#5185 = DIRECTION ( 'NONE',  ( -1.000000000000000000, 0.000000000000000000, 1.224646799147353207E-16 ) ) ;
#5186 = ORIENTED_EDGE ( 'NONE', *, *, #19179, .F. ) ;
#5187 = CIRCLE ( 'NONE', #14254, 8.105212085995399107 ) ;
#5188 = ADVANCED_FACE ( 'NONE', ( #12579 ), #12675, .F. ) ;
#5189 = DIRECTION ( 'NONE',  ( -0.000000000000000000, -0.000000000000000000, -1.000000000000000000 ) ) ;
#5190 = CARTESIAN_POINT ( 'NONE',  ( -0.5276280594146446346, 4.314175951381965746, -3.320322319201721495 ) ) ;
#5191 = EDGE_CURVE ( 'NONE', #13489, #7050, #5772, .T. ) ;
#5192 = ADVANCED_FACE ( 'NONE', ( #4153 ), #10117, .F. ) ;
#5193 = CARTESIAN_POINT ( 'NONE',  ( 6.244297270354684848, -1.798312406574552930E-11, -5.105276777067894400 ) ) ;
#5194 = DIRECTION ( 'NONE',  ( 0.000000000000000000, 1.000000000000000000, 0.000000000000000000 ) ) ;
#5195 = EDGE_CURVE ( 'NONE', #3513, #13956, #11379, .T. ) ;
#5196 = CARTESIAN_POINT ( 'NONE',  ( 0.000000000000000000, 0.000000000000000000, 15.00000000000000000 ) ) ;
#5197 = CARTESIAN_POINT ( 'NONE',  ( 43.33558569842703179, 65.09948385550239891, -2.141517661632099223 ) ) ;
#5198 = LINE ( 'NONE', #6672, #10994 ) ;
#5199 = CARTESIAN_POINT ( 'NONE',  ( 45.27934281921075410, 63.29948385550240175, -6.458785618021043895 ) ) ;
#5200 = CARTESIAN_POINT ( 'NONE',  ( 55.94051828345053679, 59.20051614449766220, 4.345558710429044069 ) ) ;
#5201 = ADVANCED_FACE ( 'NONE', ( #2399 ), #11387, .F. ) ;
#5202 = DIRECTION ( 'NONE',  ( -1.000000000000000000, -0.000000000000000000, -0.000000000000000000 ) ) ;
#5203 = CARTESIAN_POINT ( 'NONE',  ( 6.390983399715591595, 2.822795037344616897, -5.110775575965828210 ) ) ;
#5204 = AXIS2_PLACEMENT_3D ( 'NONE', #13538, #12059, #15001 ) ;
#5205 = CARTESIAN_POINT ( 'NONE',  ( 0.000000000000000000, 0.000000000000000000, 0.000000000000000000 ) ) ;
#5206 = ORIENTED_EDGE ( 'NONE', *, *, #12263, .F. ) ;
#5207 = CYLINDRICAL_SURFACE ( 'NONE', #7191, 20.00000000000000000 ) ;
#5208 = CARTESIAN_POINT ( 'NONE',  ( 56.65037692655921120, 51.10051614449766078, 2.184720259617097593 ) ) ;
#5209 = EDGE_CURVE ( 'NONE', #4677, #17411, #6885, .T. ) ;
#5210 = CIRCLE ( 'NONE', #16512, 4.799999999999999822 ) ;
#5211 = CARTESIAN_POINT ( 'NONE',  ( 4.175572532730931208, -2.061029303918052946, 3.569807470274390493 ) ) ;
#5212 = ADVANCED_FACE ( 'NONE', ( #17396 ), #17598, .T. ) ;
#5213 = CARTESIAN_POINT ( 'NONE',  ( 55.11928596558036020, 44.77036257738321012, -5.000000000000000888 ) ) ;
#5214 = ORIENTED_EDGE ( 'NONE', *, *, #13247, .F. ) ;
#5215 = DIRECTION ( 'NONE',  ( -0.000000000000000000, -0.000000000000000000, -1.000000000000000000 ) ) ;
#5216 = AXIS2_PLACEMENT_3D ( 'NONE', #18382, #429, #10898 ) ;
#5217 = CARTESIAN_POINT ( 'NONE',  ( -65.14999999999996305, 32.50000000000001421, 15.00000000000000000 ) ) ;
#5218 = DIRECTION ( 'NONE',  ( -0.04542589977017699732, 0.9989677110047501252, 0.000000000000000000 ) ) ;
#5219 = CARTESIAN_POINT ( 'NONE',  ( 5.599999999999999645, 2.020725942163688504, 3.500000000000000000 ) ) ;
#5220 = CARTESIAN_POINT ( 'NONE',  ( 1.171083334267915221, -24.65495046420793201, 9.000000000000000000 ) ) ;
#5221 = CARTESIAN_POINT ( 'NONE',  ( 57.60143344285435774, 59.10051614449766078, 2.493737253992045044 ) ) ;
#5222 = CARTESIAN_POINT ( 'NONE',  ( 55.71335778527780036, 60.90051614449766504, -1.832500667257213056 ) ) ;
#5223 = DIRECTION ( 'NONE',  ( 0.000000000000000000, 0.000000000000000000, 1.000000000000000000 ) ) ;
#5224 = CARTESIAN_POINT ( 'NONE',  ( 75.00000000000002842, -1.000000000000000000, 6.000000000000001776 ) ) ;
#5225 = EDGE_LOOP ( 'NONE', ( #1325, #450, #9826, #16567 ) ) ;
#5226 = CIRCLE ( 'NONE', #547, 2.149999999999999023 ) ;
#5227 = EDGE_LOOP ( 'NONE', ( #11023, #7444, #11115, #18862 ) ) ;
#5228 = ORIENTED_EDGE ( 'NONE', *, *, #8449, .F. ) ;
#5229 = DIRECTION ( 'NONE',  ( 1.000000000000000000, 0.000000000000000000, 0.000000000000000000 ) ) ;
#5230 = AXIS2_PLACEMENT_3D ( 'NONE', #16764, #194, #6358 ) ;
#5231 = VERTEX_POINT ( 'NONE', #18875 ) ;
#5232 = CARTESIAN_POINT ( 'NONE',  ( 3.961557105776161158, -1.423285172354515016, 3.500000000000000444 ) ) ;
#5233 = ORIENTED_EDGE ( 'NONE', *, *, #12425, .T. ) ;
#5234 = CYLINDRICAL_SURFACE ( 'NONE', #3170, 12.49999999999999645 ) ;
#5235 = ADVANCED_FACE ( 'NONE', ( #19271, #5510 ), #2693, .T. ) ;
#5236 = CARTESIAN_POINT ( 'NONE',  ( 43.34962307344081012, 56.89948385550240317, 2.184720259617164650 ) ) ;
#5237 = VERTEX_POINT ( 'NONE', #16019 ) ;
#5238 = ADVANCED_FACE ( 'NONE', ( #14523 ), #15915, .F. ) ;
#5239 = CARTESIAN_POINT ( 'NONE',  ( -1.655952806101422814, 3.662737355149034979, -7.623296525288699970E-18 ) ) ;
#5240 = ORIENTED_EDGE ( 'NONE', *, *, #15055, .T. ) ;
#5241 = TOROIDAL_SURFACE ( 'NONE', #1502, 2.200000000000001066, 0.2000000000000000111 ) ;
#5242 = CARTESIAN_POINT ( 'NONE',  ( 41.58830220609386430, 54.99948385550239749, 0.02388180880523263147 ) ) ;
#5243 = PLANE ( 'NONE',  #130 ) ;
#5244 = AXIS2_PLACEMENT_3D ( 'NONE', #8249, #11578, #11478 ) ;
#5245 = CARTESIAN_POINT ( 'NONE',  ( 53.54508667620428497, 46.29948385550240886, 4.840751629271157874 ) ) ;
#5246 = EDGE_CURVE ( 'NONE', #1750, #10122, #18934, .T. ) ;
#5247 = CARTESIAN_POINT ( 'NONE',  ( 0.9996874511566102850, -0.02500000000000036915, 0.000000000000000000 ) ) ;
#5248 = AXIS2_PLACEMENT_3D ( 'NONE', #647, #6911, #12900 ) ;
#5249 = CARTESIAN_POINT ( 'NONE',  ( 57.36023556966787851, 59.00051614449765935, 0.02388180880515038476 ) ) ;
#5250 = CARTESIAN_POINT ( 'NONE',  ( 48.07319477248768180, 64.59948385550241312, 6.007379884777225953 ) ) ;
#5251 = CARTESIAN_POINT ( 'NONE',  ( 47.70284917648453415, 59.39948385550241028, -6.992620115222774047 ) ) ;
#5252 = DIRECTION ( 'NONE',  ( 0.000000000000000000, 0.000000000000000000, 1.000000000000000000 ) ) ;
#5253 = DIRECTION ( 'NONE',  ( 1.000000000000000000, 0.000000000000000000, 0.000000000000000000 ) ) ;
#5254 = ORIENTED_EDGE ( 'NONE', *, *, #5301, .T. ) ;
#5255 = AXIS2_PLACEMENT_3D ( 'NONE', #14942, #15045, #1522 ) ;
#5256 = ORIENTED_EDGE ( 'NONE', *, *, #15871, .F. ) ;
#5257 = FACE_BOUND ( 'NONE', #15200, .T. ) ;
#5258 = VERTEX_POINT ( 'NONE', #7080 ) ;
#5259 = EDGE_CURVE ( 'NONE', #4866, #16750, #15782, .T. ) ;
#5260 = AXIS2_PLACEMENT_3D ( 'NONE', #4135, #8633, #2679 ) ;
#5261 = CARTESIAN_POINT ( 'NONE',  ( 52.29715082351547295, 60.39948385550239607, 6.992620115222774047 ) ) ;
#5262 = CARTESIAN_POINT ( 'NONE',  ( -154.9999999999999716, -14.99999999999999645, 9.000000000000000000 ) ) ;
#5263 = VERTEX_POINT ( 'NONE', #14330 ) ;
#5264 = EDGE_LOOP ( 'NONE', ( #12609, #6249, #3942 ) ) ;
#5265 = DIRECTION ( 'NONE',  ( 1.000000000000000000, 0.000000000000000000, 0.000000000000000000 ) ) ;
#5266 = ADVANCED_FACE ( 'NONE', ( #7181 ), #3858, .F. ) ;
#5267 = EDGE_LOOP ( 'NONE', ( #14667, #16805, #5651, #17818 ) ) ;
#5268 = CARTESIAN_POINT ( 'NONE',  ( 54.09612160359792199, 63.30051614449766362, 5.676469297603124353 ) ) ;
#5269 = ORIENTED_EDGE ( 'NONE', *, *, #11074, .F. ) ;
#5270 = CARTESIAN_POINT ( 'NONE',  ( 44.03140696652192787, 47.19948385550240744, -4.306917132069425058 ) ) ;
#5271 = CARTESIAN_POINT ( 'NONE',  ( 4.000000000000000888, 1.563622288139206118, -0.2253451193528334950 ) ) ;
#5272 = CARTESIAN_POINT ( 'NONE',  ( 55.11794222512599362, 62.80051614449766362, -3.688883143319583446 ) ) ;
#5273 = CARTESIAN_POINT ( 'NONE',  ( -149.0000000000000000, -14.99999999999999645, 9.000000000000000000 ) ) ;
#5274 = COLOUR_RGB ( '',1.000000000000000000, 0.9490196078431372140, 0.9098039215686274384 ) ;
#5275 = AXIS2_PLACEMENT_3D ( 'NONE', #1168, #1073, #7042 ) ;
#5276 = DIRECTION ( 'NONE',  ( 1.000000000000000000, 0.000000000000000000, 0.000000000000000000 ) ) ;
#5277 = CARTESIAN_POINT ( 'NONE',  ( -9.999999999999998224, 15.00000000000001776, -15.00000000000000000 ) ) ;
#5278 =( GEOMETRIC_REPRESENTATION_CONTEXT ( 3 ) GLOBAL_UNCERTAINTY_ASSIGNED_CONTEXT ( ( #475 ) ) GLOBAL_UNIT_ASSIGNED_CONTEXT ( ( #13517, #18328, #10556 ) ) REPRESENTATION_CONTEXT ( 'NONE', 'WORKASPACE' ) );
#5279 = ORIENTED_EDGE ( 'NONE', *, *, #1914, .F. ) ;
#5280 = ORIENTED_EDGE ( 'NONE', *, *, #11285, .T. ) ;
#5281 = CARTESIAN_POINT ( 'NONE',  ( 4.204115023516791005, -1.660442669500199919, -3.602151381774560068 ) ) ;
#5282 =( LENGTH_UNIT ( ) NAMED_UNIT ( * ) SI_UNIT ( .MILLI., .METRE. ) );
#5283 = ORIENTED_EDGE ( 'NONE', *, *, #11074, .T. ) ;
#5284 = CARTESIAN_POINT ( 'NONE',  ( 10.00000000000000000, 15.00000000000001776, -9.999999999999998224 ) ) ;
#5285 = AXIS2_PLACEMENT_3D ( 'NONE', #7909, #4882, #18137 ) ;
#5286 = DIRECTION ( 'NONE',  ( -0.000000000000000000, -0.000000000000000000, 1.000000000000000000 ) ) ;
#5287 = EDGE_LOOP ( 'NONE', ( #271, #13766 ) ) ;
#5288 = CARTESIAN_POINT ( 'NONE',  ( 0.4465819873852049926, -5.773502691896263528, -3.127607256515468906E-17 ) ) ;
#5289 = AXIS2_PLACEMENT_3D ( 'NONE', #17183, #12947, #802 ) ;
#5290 = CARTESIAN_POINT ( 'NONE',  ( -2.354826896168714434, -6.962563485461402024, -1.000000000000000000 ) ) ;
#5291 = DIRECTION ( 'NONE',  ( 1.000000000000000000, 0.000000000000000000, 0.000000000000000000 ) ) ;
#5292 = DIRECTION ( 'NONE',  ( 0.000000000000000000, 1.000000000000000000, 0.000000000000000000 ) ) ;
#5293 = CARTESIAN_POINT ( 'NONE',  ( 51.92680522751233951, 49.59948385550241312, -6.007379884777223289 ) ) ;
#5294 = DIRECTION ( 'NONE',  ( -0.000000000000000000, 0.000000000000000000, 1.000000000000000000 ) ) ;
#5295 = CARTESIAN_POINT ( 'NONE',  ( 50.02271294988512551, 48.49948385550240459, 7.000000000000000888 ) ) ;
#5296 = VECTOR ( 'NONE', #3386, 1000.000000000000000 ) ;
#5297 = CARTESIAN_POINT ( 'NONE',  ( 52.25172492374527877, 59.40051614449765083, 7.007379884777203749 ) ) ;
#5298 = CIRCLE ( 'NONE', #6245, 5.999999999999977796 ) ;
#5299 = LINE ( 'NONE', #999, #11197 ) ;
#5300 = CARTESIAN_POINT ( 'NONE',  ( 6.362374563308228481, 5.433808049139812191, -0.8060918076009558897 ) ) ;
#5301 = EDGE_CURVE ( 'NONE', #16254, #8294, #2327, .T. ) ;
#5302 = DIRECTION ( 'NONE',  ( -9.858538378746663627E-23, 5.031452844637890958E-23, -1.000000000000000000 ) ) ;
#5303 = EDGE_LOOP ( 'NONE', ( #8693, #15482, #775, #19219, #8129 ) ) ;
#5304 = PRODUCT_DEFINITION ( 'UNKNOWN', '', #11035, #3044 ) ;
#5305 = DIRECTION ( 'NONE',  ( -0.8571673013836855759, 0.000000000000000000, -0.5150380737757258576 ) ) ;
#5306 = EDGE_CURVE ( 'NONE', #1569, #2487, #13161, .T. ) ;
#5307 = CARTESIAN_POINT ( 'NONE',  ( 2.449293598294706513E-15, -20.00000000000000000, -20.00000000000000000 ) ) ;
#5308 = CARTESIAN_POINT ( 'NONE',  ( 52.29715082351539479, 50.60051614449766078, -6.992620115222796251 ) ) ;
#5309 = AXIS2_PLACEMENT_3D ( 'NONE', #7070, #2685, #16007 ) ;
#5310 = EDGE_CURVE ( 'NONE', #2665, #12330, #11072, .T. ) ;
#5311 = EDGE_CURVE ( 'NONE', #8220, #15181, #9503, .T. ) ;
#5312 = DIRECTION ( 'NONE',  ( -1.000000000000000000, 0.000000000000000000, 1.224646799147353207E-16 ) ) ;
#5313 = CARTESIAN_POINT ( 'NONE',  ( -129.9999999999999716, -14.99999999999999645, -9.000000000000000000 ) ) ;
#5314 = ORIENTED_EDGE ( 'NONE', *, *, #16458, .F. ) ;
#5315 = CARTESIAN_POINT ( 'NONE',  ( 4.158921614371307918, -1.986121848748762186, 3.559936047944509241 ) ) ;
#5316 = CARTESIAN_POINT ( 'NONE',  ( 45.60000000000000142, 0.000000000000000000, 0.000000000000000000 ) ) ;
#5317 = EDGE_CURVE ( 'NONE', #1251, #6799, #2660, .T. ) ;
#5318 = DIRECTION ( 'NONE',  ( -1.000000000000000000, 0.000000000000000000, 0.000000000000000000 ) ) ;
#5319 = AXIS2_PLACEMENT_3D ( 'NONE', #747, #5444, #5253 ) ;
#5320 = DIRECTION ( 'NONE',  ( 1.000000000000000000, 0.000000000000000000, -0.000000000000000000 ) ) ;
#5321 = CARTESIAN_POINT ( 'NONE',  ( 56.81924384183011512, 48.19948385550240744, 4.924951120819313743 ) ) ;
#5322 = CARTESIAN_POINT ( 'NONE',  ( -1.150000000000001688, 0.000000000000000000, 0.000000000000000000 ) ) ;
#5323 = CARTESIAN_POINT ( 'NONE',  ( 53.50833635130544508, 59.30051614449766362, 4.867452303228181343 ) ) ;
#5324 = DIRECTION ( 'NONE',  ( 0.000000000000000000, 0.000000000000000000, 1.000000000000000000 ) ) ;
#5325 = CARTESIAN_POINT ( 'NONE',  ( -154.9999999999999716, -6.999999999999993783, -15.00000000000000000 ) ) ;
#5326 = CIRCLE ( 'NONE', #15664, 0.7499999999999997780 ) ;
#5328 = ORIENTED_EDGE ( 'NONE', *, *, #17793, .T. ) ;
#5327 = EDGE_CURVE ( 'NONE', #16340, #5943, #7644, .T. ) ;
#5329 = EDGE_CURVE ( 'NONE', #14765, #162, #10899, .T. ) ;
#5330 = ORIENTED_EDGE ( 'NONE', *, *, #4137, .T. ) ;
#5331 = CIRCLE ( 'NONE', #5657, 0.9999999999999993339 ) ;
#5332 = CIRCLE ( 'NONE', #10334, 2.649999999999988365 ) ;
#5333 = EDGE_LOOP ( 'NONE', ( #6052, #11619, #8224, #15688 ) ) ;
#5334 = DIRECTION ( 'NONE',  ( 0.000000000000000000, 0.000000000000000000, 1.000000000000000000 ) ) ;
#5335 = EDGE_LOOP ( 'NONE', ( #2044, #1647 ) ) ;
#5336 = B_SPLINE_CURVE_WITH_KNOTS ( 'NONE', 3,
 ( #10393, #10580, #9015, #204, #16393, #17866 ),
 .UNSPECIFIED., .F., .F.,
 ( 4, 2, 4 ),
 ( 0.002452478801916376308, 0.003676905084148007850, 0.004901331366379639391 ),
 .UNSPECIFIED. ) ;
#5337 = CARTESIAN_POINT ( 'NONE',  ( 3.958491816111018746, 1.406739583089935186, 3.500000000000000000 ) ) ;
#5338 = VECTOR ( 'NONE', #18186, 1000.000000000000000 ) ;
#5339 = ORIENTED_EDGE ( 'NONE', *, *, #2841, .F. ) ;
#5340 = LINE ( 'NONE', #2517, #6293 ) ;
#5341 = CARTESIAN_POINT ( 'NONE',  ( 55.96859303347805081, 58.19948385550240744, 4.306917132069425058 ) ) ;
#5342 = ORIENTED_EDGE ( 'NONE', *, *, #9144, .F. ) ;
#5343 = CARTESIAN_POINT ( 'NONE',  ( 0.000000000000000000, 0.000000000000000000, -5.000000000000000000 ) ) ;
#5344 = VERTEX_POINT ( 'NONE', #12074 ) ;
#5345 = CARTESIAN_POINT ( 'NONE',  ( 42.39856655714566358, 50.89948385550240317, 2.493737253992119207 ) ) ;
#5346 = CONICAL_SURFACE ( 'NONE', #6287, 4.000000000000000000, 0.8911886515913786111 ) ;
#5347 = CYLINDRICAL_SURFACE ( 'NONE', #5755, 20.00000000000000000 ) ;
#5348 = CARTESIAN_POINT ( 'NONE',  ( 50.02271294988511841, 52.49948385550241170, 6.000000000000000888 ) ) ;
#5349 = DIRECTION ( 'NONE',  ( -1.000000000000000000, 0.000000000000000000, 0.000000000000000000 ) ) ;
#5350 = DIRECTION ( 'NONE',  ( 1.000000000000000000, 0.000000000000000000, 0.000000000000000000 ) ) ;
#5351 = VECTOR ( 'NONE', #10747, 1000.000000000000000 ) ;
#5352 = VECTOR ( 'NONE', #19385, 1000.000000000000000 ) ;
#5353 = CARTESIAN_POINT ( 'NONE',  ( 45.31609314410960820, 46.30051614449766362, -6.485486291978072693 ) ) ;
#5354 = CARTESIAN_POINT ( 'NONE',  ( 56.30877334542961421, 45.00051614449765225, 0.02388180880515774693 ) ) ;
#5355 = CARTESIAN_POINT ( 'NONE',  ( 0.5000000000000000000, -6.429618962271402616, -1.000000000000000000 ) ) ;
#5356 = DIRECTION ( 'NONE',  ( 1.000000000000000000, 0.000000000000000000, 0.000000000000000000 ) ) ;
#5357 = ORIENTED_EDGE ( 'NONE', *, *, #14178, .T. ) ;
#5358 = ORIENTED_EDGE ( 'NONE', *, *, #12392, .T. ) ;
#5359 = PLANE ( 'NONE',  #3725 ) ;
#5360 = ORIENTED_EDGE ( 'NONE', *, *, #6450, .T. ) ;
#5361 = CARTESIAN_POINT ( 'NONE',  ( 54.13287192849676188, 56.29948385550240175, 5.649768623646098220 ) ) ;
#5362 = CARTESIAN_POINT ( 'NONE',  ( 3.973110223767137850, 2.263269463293572928E-11, 3.565797985667434222 ) ) ;
#5363 = VECTOR ( 'NONE', #16546, 1000.000000000000000 ) ;
#5364 = ORIENTED_EDGE ( 'NONE', *, *, #2247, .F. ) ;
#5365 = AXIS2_PLACEMENT_3D ( 'NONE', #8165, #6792, #3862 ) ;
#5366 = ORIENTED_EDGE ( 'NONE', *, *, #17787, .T. ) ;
#5367 = DIRECTION ( 'NONE',  ( 1.000000000000000000, 0.000000000000000000, 0.000000000000000000 ) ) ;
#5368 = ORIENTED_EDGE ( 'NONE', *, *, #16233, .T. ) ;
#5369 = DIRECTION ( 'NONE',  ( 1.000000000000000000, 0.000000000000000000, 0.000000000000000000 ) ) ;
#5370 = ORIENTED_EDGE ( 'NONE', *, *, #14851, .T. ) ;
#5371 = CARTESIAN_POINT ( 'NONE',  ( 43.33558569842703179, 53.09948385550240602, -2.141517661632099223 ) ) ;
#5372 = DIRECTION ( 'NONE',  ( 1.000000000000000000, 0.000000000000000000, 0.000000000000000000 ) ) ;
#5373 = CARTESIAN_POINT ( 'NONE',  ( 48.07319477248762496, 62.40051614449765793, -6.007379884777208190 ) ) ;
#5374 = DIRECTION ( 'NONE',  ( 1.000000000000000000, 0.000000000000000000, 0.000000000000000000 ) ) ;
#5375 = EDGE_CURVE ( 'NONE', #10468, #9062, #16503, .T. ) ;
#5376 =( LENGTH_UNIT ( ) NAMED_UNIT ( * ) SI_UNIT ( .MILLI., .METRE. ) );
#5377 = PLANE ( 'NONE',  #648 ) ;
#5378 = ADVANCED_FACE ( 'NONE', ( #7569 ), #2974, .F. ) ;
#5379 = PRODUCT_DEFINITION_SHAPE ( 'NONE', 'NONE',  #19423 ) ;
#5380 = CIRCLE ( 'NONE', #18853, 20.00000000000000000 ) ;
#5381 = ORIENTED_EDGE ( 'NONE', *, *, #12215, .T. ) ;
#5382 = ORIENTED_EDGE ( 'NONE', *, *, #14903, .F. ) ;
#5383 = CARTESIAN_POINT ( 'NONE',  ( 3.999999999999998224, 2.472263674411418588, -3.687027874309861897 ) ) ;
#5384 =( LENGTH_UNIT ( ) NAMED_UNIT ( * ) SI_UNIT ( .MILLI., .METRE. ) );
#5385 = PLANE ( 'NONE',  #5872 ) ;
#5386 =( NAMED_UNIT ( * ) SI_UNIT ( $, .STERADIAN. ) SOLID_ANGLE_UNIT ( ) );
#5387 = ORIENTED_EDGE ( 'NONE', *, *, #17679, .F. ) ;
#5388 = DIRECTION ( 'NONE',  ( 0.000000000000000000, 0.000000000000000000, -1.000000000000000000 ) ) ;
#5389 = VERTEX_POINT ( 'NONE', #15119 ) ;
#5390 = CARTESIAN_POINT ( 'NONE',  ( 14.14213562373095101, -25.00000000000000711, -20.00000000000000000 ) ) ;
#5391 = DIRECTION ( 'NONE',  ( 0.000000000000000000, 0.000000000000000000, -1.000000000000000000 ) ) ;
#5392 = CARTESIAN_POINT ( 'NONE',  ( 46.45491332379572924, 65.29948385550241596, -4.840751629271157874 ) ) ;
#5393 = CARTESIAN_POINT ( 'NONE',  ( -17.79870116617249209, -10.87825472854619413, -9.000000000000000000 ) ) ;
#5394 = DIRECTION ( 'NONE',  ( 0.000000000000000000, 0.000000000000000000, 1.000000000000000000 ) ) ;
#5395 = CARTESIAN_POINT ( 'NONE',  ( 44.28664221472220675, 51.09948385550240602, -1.832500667257165317 ) ) ;
#5396 = DIRECTION ( 'NONE',  ( 0.3420201433256622736, 0.000000000000000000, -0.9396926207859106484 ) ) ;
#5397 = CARTESIAN_POINT ( 'NONE',  ( 43.18075615816989199, 65.19948385550240744, -4.924951120819313743 ) ) ;
#5398 = CARTESIAN_POINT ( 'NONE',  ( 47.42335538002180328, 50.40051614449766504, -8.007379884777206414 ) ) ;
#5399 = VECTOR ( 'NONE', #8579, 1000.000000000000000 ) ;
#5400 = DIRECTION ( 'NONE',  ( 1.000000000000000000, 0.000000000000000000, 0.000000000000000000 ) ) ;
#5401 = DIRECTION ( 'NONE',  ( 0.000000000000000000, 0.000000000000000000, 1.000000000000000000 ) ) ;
#5402 =( BOUNDED_CURVE ( )  B_SPLINE_CURVE ( 2, ( #3015, #13202, #10441, #4283, #11820, #16250, #12108, #2826, #18117, #8976, #13393, #14665, #17925, #4679, #18018, #16351, #8881, #10639, #14863, #19313, #14961, #19216, #11721, #14763, #1345, #7319, #13295, #5851, #4579, #17825, #4384, #10348, #1442, #4484, #1538, #10535, #15065, #1732, #15346, #3491, #3213, #360, #1826, #8077, #14053, #3300, #6234, #13955, #5140, #15154, #10735, #9175, #3581, #12397, #18502, #15537, #2115, #17027, #7698, #6333, #13676, #7893, #16828, #254, #11111, #18601, #12489, #1929, #539, #13866, #3391, #12207, #16927, #9257, #18220, #4773, #9353, #6613, #5049, #15440, #16735, #6511, #15246, #7794, #2020, #636, #13773, #7982, #12305, #12592, #18308, #4864, #10826, #9456, #446, #11020, #9545, #6418, #18406, #4948, #10921, #5428, #12791, #931, #3779, #9641, #9932, #14347, #18792, #18692, #15932, #11404, #17410, #9742, #5236, #6902, #12890, #1035, #3969, #6707, #3873, #8269, #2518, #14248, #832, #11313, #9832, #5341, #8368, #3676, #17317, #15833, #2417, #15737, #8474, #12690, #18893, #11211, #17217, #14454, #6803, #6998, #12977, #18985, #2316, #5524, #11499, #17509, #4069, #17119, #15638, #2220, #8178, #14151, #734, #4728, #13637, #18172, #7657, #3257, #7465, #10692, #1690, #11973, #13731, #12264, #16594, #212, #1593, #4632, #23, #15303, #13446, #9217, #14916, #13827, #6192, #6011, #10880, #17977, #16886, #3351, #9130, #12164, #4535, #18265, #10494, #6372, #10592, #16498, #3070, #16693, #15207, #6099, #12068, #7755, #119, #18070, #13546, #407, #12352 ),
 .UNSPECIFIED., .F., .F. ) 
 B_SPLINE_CURVE_WITH_KNOTS ( ( 3, 2, 2, 2, 2, 2, 2, 2, 2, 2, 2, 2, 2, 2, 2, 2, 2, 2, 2, 2, 2, 2, 2, 2, 2, 2, 2, 2, 2, 2, 2, 2, 2, 2, 2, 2, 2, 2, 2, 2, 2, 2, 2, 2, 2, 2, 2, 2, 2, 2, 2, 2, 2, 2, 2, 2, 2, 2, 2, 2, 2, 2, 2, 2, 2, 2, 2, 2, 2, 2, 2, 2, 2, 2, 2, 2, 2, 2, 2, 2, 2, 2, 2, 2, 2, 2, 2, 2, 2, 2, 2, 2, 2, 2, 2, 2, 2, 2, 2, 2, 3 ),
 ( 0.000000000000000000, 0.01000000000000000021, 0.02000000000000000042, 0.02999999999999999889, 0.04000000000000000083, 0.05000000000000000278, 0.05999999999999999778, 0.07000000000000000666, 0.08000000000000000167, 0.08999999999999999667, 0.1000000000000000056, 0.1100000000000000006, 0.1199999999999999956, 0.1300000000000000044, 0.1400000000000000133, 0.1499999999999999944, 0.1600000000000000033, 0.1700000000000000122, 0.1799999999999999933, 0.1900000000000000022, 0.2000000000000000111, 0.2099999999999999922, 0.2200000000000000011, 0.2300000000000000100, 0.2399999999999999911, 0.2500000000000000000, 0.2600000000000000089, 0.2700000000000000178, 0.2800000000000000266, 0.2899999999999999800, 0.2999999999999999889, 0.3099999999999999978, 0.3200000000000000067, 0.3300000000000000155, 0.3400000000000000244, 0.3499999999999999778, 0.3599999999999999867, 0.3699999999999999956, 0.3800000000000000044, 0.3900000000000000133, 0.4000000000000000222, 0.4099999999999999756, 0.4199999999999999845, 0.4299999999999999933, 0.4400000000000000022, 0.4500000000000000111, 0.4600000000000000200, 0.4699999999999999734, 0.4799999999999999822, 0.4899999999999999911, 0.5000000000000000000, 0.5100000000000000089, 0.5200000000000000178, 0.5300000000000000266, 0.5400000000000000355, 0.5500000000000000444, 0.5600000000000000533, 0.5699999999999999512, 0.5799999999999999600, 0.5899999999999999689, 0.5999999999999999778, 0.6099999999999999867, 0.6199999999999999956, 0.6300000000000000044, 0.6400000000000000133, 0.6500000000000000222, 0.6600000000000000311, 0.6700000000000000400, 0.6800000000000000488, 0.6899999999999999467, 0.6999999999999999556, 0.7099999999999999645, 0.7199999999999999734, 0.7299999999999999822, 0.7399999999999999911, 0.7500000000000000000, 0.7600000000000000089, 0.7700000000000000178, 0.7800000000000000266, 0.7900000000000000355, 0.8000000000000000444, 0.8100000000000000533, 0.8199999999999999512, 0.8299999999999999600, 0.8399999999999999689, 0.8499999999999999778, 0.8599999999999999867, 0.8699999999999999956, 0.8800000000000000044, 0.8900000000000000133, 0.9000000000000000222, 0.9100000000000000311, 0.9200000000000000400, 0.9300000000000000488, 0.9399999999999999467, 0.9499999999999999556, 0.9599999999999999645, 0.9699999999999999734, 0.9799999999999999822, 0.9899999999999999911, 1.000000000000000000 ),
 .UNSPECIFIED. ) 
 CURVE ( )  GEOMETRIC_REPRESENTATION_ITEM ( )  RATIONAL_B_SPLINE_CURVE ( ( 1.000000000000000000, 0.9510565162951535312, 1.000000000000000000, 0.9510565162951535312, 1.000000000000000000, 0.9510565162951535312, 1.000000000000000000, 0.9510565162951535312, 1.000000000000000000, 0.9510565162951535312, 1.000000000000000000, 0.9510565162951535312, 1.000000000000000000, 0.9510565162951535312, 1.000000000000000000, 0.9510565162951535312, 1.000000000000000000, 0.9510565162951535312, 1.000000000000000000, 0.9510565162951535312, 1.000000000000000000, 0.9510565162951535312, 1.000000000000000000, 0.9510565162951535312, 1.000000000000000000, 0.9510565162951535312, 1.000000000000000000, 0.9510565162951535312, 1.000000000000000000, 0.9510565162951535312, 1.000000000000000000, 0.9510565162951535312, 1.000000000000000000, 0.9510565162951535312, 1.000000000000000000, 0.9510565162951535312, 1.000000000000000000, 0.9510565162951535312, 1.000000000000000000, 0.9510565162951535312, 1.000000000000000000, 0.9510565162951535312, 1.000000000000000000, 0.9510565162951535312, 1.000000000000000000, 0.9510565162951535312, 1.000000000000000000, 0.9510565162951535312, 1.000000000000000000, 0.9510565162951535312, 1.000000000000000000, 0.9510565162951535312, 1.000000000000000000, 0.9510565162951535312, 1.000000000000000000, 0.9510565162951535312, 1.000000000000000000, 0.9510565162951535312, 1.000000000000000000, 0.9510565162951535312, 1.000000000000000000, 0.9510565162951535312, 1.000000000000000000, 0.9510565162951535312, 1.000000000000000000, 0.9510565162951535312, 1.000000000000000000, 0.9510565162951535312, 1.000000000000000000, 0.9510565162951535312, 1.000000000000000000, 0.9510565162951535312, 1.000000000000000000, 0.9510565162951535312, 1.000000000000000000, 0.9510565162951535312, 1.000000000000000000, 0.9510565162951535312, 1.000000000000000000, 0.9510565162951535312, 1.000000000000000000, 0.9510565162951535312, 1.000000000000000000, 0.9510565162951535312, 1.000000000000000000, 0.9510565162951535312, 1.000000000000000000, 0.9510565162951535312, 1.000000000000000000, 0.9510565162951535312, 1.000000000000000000, 0.9510565162951535312, 1.000000000000000000, 0.9510565162951535312, 1.000000000000000000, 0.9510565162951535312, 1.000000000000000000, 0.9510565162951535312, 1.000000000000000000, 0.9510565162951535312, 1.000000000000000000, 0.9510565162951535312, 1.000000000000000000, 0.9510565162951535312, 1.000000000000000000, 0.9510565162951535312, 1.000000000000000000, 0.9510565162951535312, 1.000000000000000000, 0.9510565162951535312, 1.000000000000000000, 0.9510565162951535312, 1.000000000000000000, 0.9510565162951535312, 1.000000000000000000, 0.9510565162951535312, 1.000000000000000000, 0.9510565162951535312, 1.000000000000000000, 0.9510565162951535312, 1.000000000000000000, 0.9510565162951535312, 1.000000000000000000, 0.9510565162951535312, 1.000000000000000000, 0.9510565162951535312, 1.000000000000000000, 0.9510565162951535312, 1.000000000000000000, 0.9510565162951535312, 1.000000000000000000, 0.9510565162951535312, 1.000000000000000000, 0.9510565162951535312, 1.000000000000000000, 0.9510565162951535312, 1.000000000000000000, 0.9510565162951535312, 1.000000000000000000, 0.9510565162951535312, 1.000000000000000000, 0.9510565162951535312, 1.000000000000000000, 0.9510565162951535312, 1.000000000000000000, 0.9510565162951535312, 1.000000000000000000, 0.9510565162951535312, 1.000000000000000000, 0.9510565162951535312, 1.000000000000000000, 0.9510565162951535312, 1.000000000000000000, 0.9510565162951535312, 1.000000000000000000, 0.9510565162951535312, 1.000000000000000000, 0.9510565162951535312, 1.000000000000000000, 0.9510565162951535312, 1.000000000000000000, 0.9510565162951535312, 1.000000000000000000, 0.9510565162951535312, 1.000000000000000000, 0.9510565162951535312, 1.000000000000000000, 0.9510565162951535312, 1.000000000000000000, 0.9510565162951535312, 1.000000000000000000, 0.9510565162951535312, 1.000000000000000000, 0.9510565162951535312, 1.000000000000000000, 0.9510565162951535312, 1.000000000000000000, 0.9510565162951535312, 1.000000000000000000, 0.9510565162951535312, 1.000000000000000000, 0.9510565162951535312, 1.000000000000000000, 0.9510565162951535312, 1.000000000000000000, 0.9510565162951535312, 1.000000000000000000, 0.9510565162951535312, 1.000000000000000000, 0.9510565162951535312, 1.000000000000000000, 0.9510565162951535312, 1.000000000000000000, 0.9510565162951535312, 1.000000000000000000, 0.9510565162951535312, 1.000000000000000000, 0.9510565162951535312, 1.000000000000000000, 0.9510565162951535312, 1.000000000000000000 ) ) 
 REPRESENTATION_ITEM ( '' )  );
#5403 = VERTEX_POINT ( 'NONE', #124 ) ;
#5404 = CARTESIAN_POINT ( 'NONE',  ( 2.449293598294706513E-15, -20.00000000000000000, 9.999999999999998224 ) ) ;
#5405 = CARTESIAN_POINT ( 'NONE',  ( 47.70284917648459810, 55.60051614449765367, 6.992620115222797139 ) ) ;
#5406 = CARTESIAN_POINT ( 'NONE',  ( -20.63749999999999574, 0.000000000000000000, -5.575000000000000178 ) ) ;
#5407 = CARTESIAN_POINT ( 'NONE',  ( 2.449293598294706513E-15, -20.00000000000000000, -20.00000000000000000 ) ) ;
#5408 = ORIENTED_EDGE ( 'NONE', *, *, #15044, .T. ) ;
#5409 = DIRECTION ( 'NONE',  ( -0.000000000000000000, 1.000000000000000000, -0.000000000000000000 ) ) ;
#5410 = CARTESIAN_POINT ( 'NONE',  ( -19.76107906696391225, -16.91783288752853665, 9.000000000000000000 ) ) ;
#5411 = EDGE_CURVE ( 'NONE', #13074, #3032, #8939, .T. ) ;
#5412 = CARTESIAN_POINT ( 'NONE',  ( -6.259644161404860030E-16, -4.618802153517027165, -5.000000000000000000 ) ) ;
#5413 = CARTESIAN_POINT ( 'NONE',  ( 45.86712807150323812, 53.29948385550240886, -5.649768623646098220 ) ) ;
#5414 = DIRECTION ( 'NONE',  ( 0.000000000000000000, 0.000000000000000000, 1.000000000000000000 ) ) ;
#5415 = CARTESIAN_POINT ( 'NONE',  ( 47.42335538002180328, 64.40051614449764372, -8.007379884777206414 ) ) ;
#5416 = CARTESIAN_POINT ( 'NONE',  ( -17.85000000000000142, -19.99999999999999289, -23.00000000000000000 ) ) ;
#5417 = CARTESIAN_POINT ( 'NONE',  ( 44.28664221472221385, 61.90051614449766504, 1.832500667257213722 ) ) ;
#5418 = DIRECTION ( 'NONE',  ( 1.000000000000000000, 0.000000000000000000, 0.000000000000000000 ) ) ;
#5419 = CARTESIAN_POINT ( 'NONE',  ( 53.50000000000000000, 4.475777889183788807E-16, -3.309499999999999886 ) ) ;
#5420 = EDGE_LOOP ( 'NONE', ( #15567, #10795, #786, #15765 ) ) ;
#5421 = ORIENTED_EDGE ( 'NONE', *, *, #8050, .T. ) ;
#5422 = DIRECTION ( 'NONE',  ( 0.000000000000000000, 0.000000000000000000, 1.000000000000000000 ) ) ;
#5423 = ORIENTED_EDGE ( 'NONE', *, *, #11783, .T. ) ;
#5424 = CARTESIAN_POINT ( 'NONE',  ( 75.00000000000000000, 40.00000000000000000, 10.00000000000000000 ) ) ;
#5425 = EDGE_CURVE ( 'NONE', #11229, #10265, #1695, .T. ) ;
#5426 = ORIENTED_EDGE ( 'NONE', *, *, #7528, .T. ) ;
#5427 = DIRECTION ( 'NONE',  ( 1.000000000000000000, 0.000000000000000000, 0.000000000000000000 ) ) ;
#5428 = CARTESIAN_POINT ( 'NONE',  ( 52.25172492374522903, 55.59948385550241312, -7.007379884777227730 ) ) ;
#5429 = EDGE_LOOP ( 'NONE', ( #17900, #11793, #10748, #67 ) ) ;
#5430 = DIRECTION ( 'NONE',  ( -0.9999670257950099561, -0.008120795692649453515, 0.000000000000000000 ) ) ;
#5431 = ORIENTED_EDGE ( 'NONE', *, *, #168, .T. ) ;
#5432 = CARTESIAN_POINT ( 'NONE',  ( 43.20883090819745576, 60.79948385550241596, 4.963592699179006473 ) ) ;
#5433 = CARTESIAN_POINT ( 'NONE',  ( -2.919722569185572480E-15, 2.859595677584338524, -2.047034997319574945 ) ) ;
#5434 = EDGE_CURVE ( 'NONE', #337, #11695, #14922, .T. ) ;
#5435 = CARTESIAN_POINT ( 'NONE',  ( 49.97728705011488870, 53.49948385550240459, -6.000000000000000888 ) ) ;
#5436 = VECTOR ( 'NONE', #7396, 1000.000000000000227 ) ;
#5437 = FACE_BOUND ( 'NONE', #14077, .T. ) ;
#5438 = ADVANCED_FACE ( 'NONE', ( #10599 ), #10408, .T. ) ;
#5439 = LINE ( 'NONE', #14644, #18733 ) ;
#5440 = CARTESIAN_POINT ( 'NONE',  ( 58.41169779390614281, 45.00051614449765225, 0.02388180880515032231 ) ) ;
#5441 = VECTOR ( 'NONE', #10017, 1000.000000000000000 ) ;
#5442 = CARTESIAN_POINT ( 'NONE',  ( 48.07319477248768180, 62.59948385550238470, 6.007379884777225953 ) ) ;
#5443 = LINE ( 'NONE', #11421, #17890 ) ;
#5444 = DIRECTION ( 'NONE',  ( 0.000000000000000000, 0.000000000000000000, 1.000000000000000000 ) ) ;
#5445 = ORIENTED_EDGE ( 'NONE', *, *, #6064, .T. ) ;
#5446 = EDGE_CURVE ( 'NONE', #14776, #16413, #13452, .T. ) ;
#5447 = EDGE_CURVE ( 'NONE', #17028, #15978, #14122, .T. ) ;
#5448 = EDGE_LOOP ( 'NONE', ( #13879, #1124, #10565, #14704 ) ) ;
#5449 = DIRECTION ( 'NONE',  ( 0.000000000000000000, 0.000000000000000000, 1.000000000000000000 ) ) ;
#5450 = VERTEX_POINT ( 'NONE', #10499 ) ;
#5451 = AXIS2_PLACEMENT_3D ( 'NONE', #17683, #11681, #5610 ) ;
#5452 = EDGE_CURVE ( 'NONE', #248, #2665, #8504, .T. ) ;
#5453 = CARTESIAN_POINT ( 'NONE',  ( 45.86712807150323812, 59.29948385550240175, -5.649768623646098220 ) ) ;
#5454 = DIRECTION ( 'NONE',  ( 0.000000000000000000, -0.000000000000000000, 1.000000000000000000 ) ) ;
#5455 = ORIENTED_EDGE ( 'NONE', *, *, #7882, .F. ) ;
#5456 = ORIENTED_EDGE ( 'NONE', *, *, #4974, .T. ) ;
#5457 = AXIS2_PLACEMENT_3D ( 'NONE', #14112, #18364, #10785 ) ;
#5458 = DIRECTION ( 'NONE',  ( -0.000000000000000000, 0.000000000000000000, 1.000000000000000000 ) ) ;
#5459 = ORIENTED_EDGE ( 'NONE', *, *, #18569, .F. ) ;
#5460 = LINE ( 'NONE', #8598, #12249 ) ;
#5461 = VERTEX_POINT ( 'NONE', #17779 ) ;
#5462 = CARTESIAN_POINT ( 'NONE',  ( 44.05948171654949874, 54.79948385550241596, 4.345558710429105354 ) ) ;
#5463 = CARTESIAN_POINT ( 'NONE',  ( 1.925929944387235853E-31, 15.00000000000001599, -9.000000000000000000 ) ) ;
#5464 = CARTESIAN_POINT ( 'NONE',  ( 55.96859303347802239, 44.80051614449767072, -4.306917132069484566 ) ) ;
#5465 = DIRECTION ( 'NONE',  ( -0.000000000000000000, -0.000000000000000000, -1.000000000000000000 ) ) ;
#5466 = SURFACE_STYLE_FILL_AREA ( #8606 ) ;
#5467 = CARTESIAN_POINT ( 'NONE',  ( -4.158233816355195955, -0.4370479853238878887, 9.000000000000000000 ) ) ;
#5468 = CIRCLE ( 'NONE', #16766, 8.000000000000007105 ) ;
#5469 = VERTEX_POINT ( 'NONE', #1600 ) ;
#5470 = ORIENTED_EDGE ( 'NONE', *, *, #18391, .T. ) ;
#5471 = DIRECTION ( 'NONE',  ( 0.03933706530295848214, -0.9992259981072103558, 7.446367396525006349E-17 ) ) ;
#5472 = VECTOR ( 'NONE', #9520, 1000.000000000000227 ) ;
#5473 = DIRECTION ( 'NONE',  ( 0.1045284632676494602, 0.9945218953682738450, 0.000000000000000000 ) ) ;
#5474 = DIRECTION ( 'NONE',  ( 1.000000000000000000, 0.000000000000000000, 0.000000000000000000 ) ) ;
#5475 = ITEM_DEFINED_TRANSFORMATION ( 'NONE', 'NONE', #18470,  #10359 ) ;
#5476 = ORIENTED_EDGE ( 'NONE', *, *, #16237, .F. ) ;
#5477 = CARTESIAN_POINT ( 'NONE',  ( 6.403457969954082785, 5.776886471390908717, -1.402224347649779865E-18 ) ) ;
#5478 = EDGE_CURVE ( 'NONE', #3135, #4627, #17603, .T. ) ;
#5479 = CIRCLE ( 'NONE', #7979, 0.7500000000000002220 ) ;
#5480 = VERTEX_POINT ( 'NONE', #3175 ) ;
#5481 = ORIENTED_EDGE ( 'NONE', *, *, #13828, .T. ) ;
#5482 = EDGE_CURVE ( 'NONE', #1879, #14662, #7662, .T. ) ;
#5483 = DIRECTION ( 'NONE',  ( -0.000000000000000000, -0.000000000000000000, 1.000000000000000000 ) ) ;
#5484 = B_SPLINE_CURVE_WITH_KNOTS ( 'NONE', 3,
 ( #46, #11993, #13565, #14740, #4653, #5827 ),
 .UNSPECIFIED., .F., .F.,
 ( 4, 2, 4 ),
 ( 0.002365888236227967761, 0.003551327329835077609, 0.004736766423442186590 ),
 .UNSPECIFIED. ) ;
#5485 = CARTESIAN_POINT ( 'NONE',  ( -2.837560373301905643E-16, 0.3423821193871246504, -3.499999999999999556 ) ) ;
#5486 = CARTESIAN_POINT ( 'NONE',  ( 44.28664221472221385, 45.90051614449766504, 1.832500667257213722 ) ) ;
#5487 = DIRECTION ( 'NONE',  ( 0.000000000000000000, -0.000000000000000000, 1.000000000000000000 ) ) ;
#5488 = CIRCLE ( 'NONE', #14238, 3.799999999999999378 ) ;
#5489 = CARTESIAN_POINT ( 'NONE',  ( -72.99999999999997158, -3.000000000000000000, -5.999999999999998224 ) ) ;
#5490 = CARTESIAN_POINT ( 'NONE',  ( 48.07319477248768180, 52.59948385550240602, 6.007379884777225953 ) ) ;
#5491 = CARTESIAN_POINT ( 'NONE',  ( 0.3126073911696427010, 4.041451884327382338, -6.521455134176256610E-17 ) ) ;
#5492 = CARTESIAN_POINT ( 'NONE',  ( 45.27934281921075410, 65.29948385550241596, -6.458785618021043895 ) ) ;
#5493 = CARTESIAN_POINT ( 'NONE',  ( 54.72065718078918906, 46.70051614449766220, -6.458785618021089192 ) ) ;
#5494 = PLANE ( 'NONE',  #12512 ) ;
#5495 = DIRECTION ( 'NONE',  ( -1.000000000000000000, 0.000000000000000000, 0.000000000000000000 ) ) ;
#5496 = CARTESIAN_POINT ( 'NONE',  ( 6.212068001623052282, 5.350125758160769962, -0.7333103599825900876 ) ) ;
#5497 = DIRECTION ( 'NONE',  ( 0.000000000000000000, 0.000000000000000000, 1.000000000000000000 ) ) ;
#5498 = ORIENTED_EDGE ( 'NONE', *, *, #7764, .T. ) ;
#5499 = CARTESIAN_POINT ( 'NONE',  ( 4.000000000000000000, 2.309401076758497151, -3.433295621305379353 ) ) ;
#5500 = AXIS2_PLACEMENT_3D ( 'NONE', #16670, #13317, #95 ) ;
#5501 = PLANE ( 'NONE',  #5309 ) ;
#5502 = CARTESIAN_POINT ( 'NONE',  ( 47.74827507625470702, 52.40051614449765083, -7.007379884777204637 ) ) ;
#5503 = CARTESIAN_POINT ( 'NONE',  ( 0.3126073911696451990, -4.041451884327386779, -1.834154111220703958E-17 ) ) ;
#5504 = CIRCLE ( 'NONE', #11125, 0.7500000000000000000 ) ;
#5505 = FACE_OUTER_BOUND ( 'NONE', #17220, .T. ) ;
#5506 = ORIENTED_EDGE ( 'NONE', *, *, #3836, .T. ) ;
#5507 = CARTESIAN_POINT ( 'NONE',  ( 0.1739375980333722760, 3.358985280702821097, 4.182066831946702479 ) ) ;
#5508 = DIRECTION ( 'NONE',  ( 0.000000000000000000, 0.000000000000000000, 1.000000000000000000 ) ) ;
#5509 = CARTESIAN_POINT ( 'NONE',  ( 56.66441430157296821, 52.09948385550240602, 2.141517661632100111 ) ) ;
#5510 = FACE_OUTER_BOUND ( 'NONE', #8020, .T. ) ;
#5511 = CARTESIAN_POINT ( 'NONE',  ( 57.60143344285435774, 63.10051614449766078, 2.493737253992045044 ) ) ;
#5512 = CYLINDRICAL_SURFACE ( 'NONE', #18865, 12.49999999999999645 ) ;
#5513 = CARTESIAN_POINT ( 'NONE',  ( 44.05948171654945611, 50.20051614449764088, -4.345558710429044069 ) ) ;
#5514 = FACE_OUTER_BOUND ( 'NONE', #3395, .T. ) ;
#5515 = CARTESIAN_POINT ( 'NONE',  ( -2.649999999999988365, 15.00000000000001599, 9.999999999999998224 ) ) ;
#5516 = ORIENTED_EDGE ( 'NONE', *, *, #18270, .T. ) ;
#5517 = ORIENTED_EDGE ( 'NONE', *, *, #14535, .F. ) ;
#5518 = DIRECTION ( 'NONE',  ( -1.000000000000000000, -0.000000000000000000, -0.000000000000000000 ) ) ;
#5519 = ORIENTED_EDGE ( 'NONE', *, *, #16002, .F. ) ;
#5520 = CARTESIAN_POINT ( 'NONE',  ( 4.030875481282487627, 1.403567514399325367, 3.500000000000000000 ) ) ;
#5521 = VECTOR ( 'NONE', #16806, 1000.000000000000114 ) ;
#5522 = ORIENTED_EDGE ( 'NONE', *, *, #5927, .T. ) ;
#5523 = CARTESIAN_POINT ( 'NONE',  ( 0.000000000000000000, 0.000000000000000000, 0.000000000000000000 ) ) ;
#5524 = CARTESIAN_POINT ( 'NONE',  ( 57.36023556966787851, 59.99948385550240459, -0.02388180880522424582 ) ) ;
#5525 = VERTEX_POINT ( 'NONE', #18179 ) ;
#5526 = CARTESIAN_POINT ( 'NONE',  ( 0.9999999999999997780, -6.008326913195983998, -0.8000000000000000444 ) ) ;
#5527 = VERTEX_POINT ( 'NONE', #4738 ) ;
#5528 = CARTESIAN_POINT ( 'NONE',  ( 43.18075615816989199, 61.19948385550241454, -4.924951120819313743 ) ) ;
#5529 = CARTESIAN_POINT ( 'NONE',  ( -74.99999999999997158, 1.000000000000000000, 6.000000000000000000 ) ) ;
#5530 = AXIS2_PLACEMENT_3D ( 'NONE', #17774, #8935, #10300 ) ;
#5531 = PRODUCT_DEFINITION_SHAPE ( 'NONE', 'NONE',  #19429 ) ;
#5532 = CARTESIAN_POINT ( 'NONE',  ( 44.28664221472220675, 49.09948385550241312, -1.832500667257165317 ) ) ;
#5533 = CARTESIAN_POINT ( 'NONE',  ( -154.9999999999999716, -14.99999999999999645, -17.00000000000000000 ) ) ;
#5534 = DIRECTION ( 'NONE',  ( -1.000000000000000000, -0.000000000000000000, -0.000000000000000000 ) ) ;
#5535 = CARTESIAN_POINT ( 'NONE',  ( 42.39856655714564226, 50.10051614449766078, -2.493737253992044156 ) ) ;
#5536 = CARTESIAN_POINT ( 'NONE',  ( 50.02271294988506156, 46.50051614449766646, -6.000000000000000888 ) ) ;
#5537 = CARTESIAN_POINT ( 'NONE',  ( 6.385552186430388133, -2.886751345948118441, 5.000000000000000888 ) ) ;
#5538 = CIRCLE ( 'NONE', #3983, 4.999999999999999112 ) ;
#5539 = DIRECTION ( 'NONE',  ( -1.000000000000000000, 1.224646799147352714E-16, 0.000000000000000000 ) ) ;
#5540 = ORIENTED_EDGE ( 'NONE', *, *, #6305, .F. ) ;
#5541 = ORIENTED_EDGE ( 'NONE', *, *, #18395, .T. ) ;
#5542 = DIRECTION ( 'NONE',  ( -0.9914448613738103822, -0.1305261922200521840, 0.000000000000000000 ) ) ;
#5543 = SURFACE_STYLE_FILL_AREA ( #3086 ) ;
#5544 = VERTEX_POINT ( 'NONE', #10699 ) ;
#5545 = EDGE_CURVE ( 'NONE', #869, #3393, #10306, .T. ) ;
#5546 = CARTESIAN_POINT ( 'NONE',  ( 55.96859303347804371, 56.19948385550241454, 4.306917132069425946 ) ) ;
#5547 = DIRECTION ( 'NONE',  ( 1.000000000000000000, 0.000000000000000000, 0.000000000000000000 ) ) ;
#5548 = CIRCLE ( 'NONE', #12126, 2.000000000000001776 ) ;
#5549 = ORIENTED_EDGE ( 'NONE', *, *, #6162, .T. ) ;
#5550 = ORIENTED_EDGE ( 'NONE', *, *, #3699, .F. ) ;
#5551 = LINE ( 'NONE', #958, #18374 ) ;
#5552 = ADVANCED_FACE ( 'NONE', ( #2886 ), #14822, .F. ) ;
#5553 = AXIS2_PLACEMENT_3D ( 'NONE', #12657, #12456, #8041 ) ;
#5554 = ORIENTED_EDGE ( 'NONE', *, *, #3634, .T. ) ;
#5555 = CARTESIAN_POINT ( 'NONE',  ( 0.000000000000000000, 4.330127018922190985, 2.500000000000005329 ) ) ;
#5556 = ORIENTED_EDGE ( 'NONE', *, *, #6027, .F. ) ;
#5557 = AXIS2_PLACEMENT_3D ( 'NONE', #19201, #17518, #16141 ) ;
#5558 = CARTESIAN_POINT ( 'NONE',  ( 1.150000000000000577, 0.000000000000000000, 0.000000000000000000 ) ) ;
#5559 = EDGE_CURVE ( 'NONE', #19337, #9539, #2287, .T. ) ;
#5560 = ADVANCED_FACE ( 'NONE', ( #3548 ), #4825, .T. ) ;
#5561 = CARTESIAN_POINT ( 'NONE',  ( 47.74827507625478518, 48.59948385550239180, 7.007379884777227730 ) ) ;
#5562 = CARTESIAN_POINT ( 'NONE',  ( 20.00000000000000000, -20.00000000000000000, -12.00000000000000000 ) ) ;
#5563 = CARTESIAN_POINT ( 'NONE',  ( 56.65037692655921120, 47.10051614449766078, 2.184720259617097593 ) ) ;
#5564 = DIRECTION ( 'NONE',  ( 0.000000000000000000, 0.000000000000000000, -1.000000000000000000 ) ) ;
#5565 = ADVANCED_FACE ( 'NONE', ( #12453 ), #1983, .T. ) ;
#5566 = CARTESIAN_POINT ( 'NONE',  ( 14.14213562373095101, -25.00000000000000711, -23.00000000000000000 ) ) ;
#5567 = CARTESIAN_POINT ( 'NONE',  ( 0.000000000000000000, 0.5192545390863916310, -1.000000000000000000 ) ) ;
#5568 = VECTOR ( 'NONE', #12577, 1000.000000000000000 ) ;
#5569 = VECTOR ( 'NONE', #4036, 1000.000000000000000 ) ;
#5570 = VERTEX_POINT ( 'NONE', #17083 ) ;
#5571 = ORIENTED_EDGE ( 'NONE', *, *, #13634, .F. ) ;
#5572 = LINE ( 'NONE', #9973, #9642 ) ;
#5573 =( NAMED_UNIT ( * ) PLANE_ANGLE_UNIT ( ) SI_UNIT ( $, .RADIAN. ) );
#5574 = EDGE_CURVE ( 'NONE', #18909, #4790, #5198, .T. ) ;
#5575 = FACE_OUTER_BOUND ( 'NONE', #16050, .T. ) ;
#5576 = EDGE_CURVE ( 'NONE', #2066, #6724, #10372, .T. ) ;
#5577 = PLANE ( 'NONE',  #10588 ) ;
#5578 = PRESENTATION_LAYER_ASSIGNMENT (  '', '', ( #15925 ) ) ;
#5579 = VERTEX_POINT ( 'NONE', #15702 ) ;
#5580 = CARTESIAN_POINT ( 'NONE',  ( -8.134732861515892921, -38.27090915285207018, 9.000000000000000000 ) ) ;
#5581 = ORIENTED_EDGE ( 'NONE', *, *, #13341, .F. ) ;
#5582 = ORIENTED_EDGE ( 'NONE', *, *, #11774, .F. ) ;
#5583 = COLOUR_RGB ( '',1.000000000000000000, 0.9490196078431372140, 0.9098039215686274384 ) ;
#5584 = VECTOR ( 'NONE', #15364, 1000.000000000000000 ) ;
#5585 = CARTESIAN_POINT ( 'NONE',  ( -14.86289650954781649, -33.38261212717723936, -9.000000000000000000 ) ) ;
#5586 = CARTESIAN_POINT ( 'NONE',  ( -154.9999999999999716, -14.99999999999999645, -9.000000000000000000 ) ) ;
#5587 = CARTESIAN_POINT ( 'NONE',  ( 46.45491332379576477, 51.70051614449765509, 4.840751629271188961 ) ) ;
#5588 = FACE_OUTER_BOUND ( 'NONE', #4227, .T. ) ;
#5589 = PLANE ( 'NONE',  #4934 ) ;
#5590 = CARTESIAN_POINT ( 'NONE',  ( 55.08986747509847248, 49.79948385550240175, -3.727524721679197572 ) ) ;
#5591 = MECHANICAL_DESIGN_GEOMETRIC_PRESENTATION_REPRESENTATION (  '', ( #1850 ), #2157 ) ;
#5592 = FACE_OUTER_BOUND ( 'NONE', #2394, .T. ) ;
#5593 = CARTESIAN_POINT ( 'NONE',  ( 41.58830220609386430, 64.99948385550240459, 0.02388180880523263147 ) ) ;
#5594 = CARTESIAN_POINT ( 'NONE',  ( 54.68390685589039890, 49.30051614449766362, 6.485486291978072693 ) ) ;
#5595 = DIRECTION ( 'NONE',  ( 1.000000000000000000, 0.000000000000000000, 0.000000000000000000 ) ) ;
#5596 = FACE_OUTER_BOUND ( 'NONE', #12693, .T. ) ;
#5597 = VECTOR ( 'NONE', #7721, 1000.000000000000114 ) ;
#5598 = AXIS2_PLACEMENT_3D ( 'NONE', #9765, #3894, #751 ) ;
#5599 = EDGE_CURVE ( 'NONE', #7384, #9761, #55, .T. ) ;
#5600 = VERTEX_POINT ( 'NONE', #9507 ) ;
#5601 = CARTESIAN_POINT ( 'NONE',  ( 2.000000000000000444, 3.464101615137754830, -3.142992957459231018 ) ) ;
#5602 = EDGE_CURVE ( 'NONE', #869, #10775, #2576, .T. ) ;
#5603 = CARTESIAN_POINT ( 'NONE',  ( 19.76107906696393357, -23.08216711247132835, 9.000000000000000000 ) ) ;
#5604 = PRESENTATION_LAYER_ASSIGNMENT (  '', '', ( #1850 ) ) ;
#5605 = CARTESIAN_POINT ( 'NONE',  ( 42.63976443033212149, 52.00051614449765935, -0.02388180880514948964 ) ) ;
#5606 = DIRECTION ( 'NONE',  ( -0.000000000000000000, -0.000000000000000000, 1.000000000000000000 ) ) ;
#5607 = DIRECTION ( 'NONE',  ( 0.000000000000000000, 0.000000000000000000, 1.000000000000000000 ) ) ;
#5608 = ORIENTED_EDGE ( 'NONE', *, *, #17496, .F. ) ;
#5609 = AXIS2_PLACEMENT_3D ( 'NONE', #42, #16126, #17896 ) ;
#5610 = DIRECTION ( 'NONE',  ( 1.000000000000000000, 0.000000000000000000, 0.000000000000000000 ) ) ;
#5611 = AXIS2_PLACEMENT_3D ( 'NONE', #10630, #13671, #18110 ) ;
#5612 = CARTESIAN_POINT ( 'NONE',  ( 47.70284917648453415, 51.39948385550238896, -6.992620115222774047 ) ) ;
#5613 = DIRECTION ( 'NONE',  ( 0.000000000000000000, 0.000000000000000000, -1.000000000000000000 ) ) ;
#5614 = CARTESIAN_POINT ( 'NONE',  ( 45.31609314410967926, 48.69948385550241454, 6.485486291978119766 ) ) ;
#5615 = CARTESIAN_POINT ( 'NONE',  ( -4.154094228333456762, 2.398367420968013253, -3.721909803043220055 ) ) ;
#5616 = CARTESIAN_POINT ( 'NONE',  ( 54.13287192849671214, 48.70051614449766220, -5.649768623646139964 ) ) ;
#5617 = EDGE_CURVE ( 'NONE', #2130, #11693, #9129, .T. ) ;
#5618 = CARTESIAN_POINT ( 'NONE',  ( 6.207541730803228575, -1.039448978216581665, 5.000000000000000888 ) ) ;
#5619 = ORIENTED_EDGE ( 'NONE', *, *, #17457, .T. ) ;
#5620 = ADVANCED_FACE ( 'NONE', ( #15406 ), #8036, .T. ) ;
#5621 = ORIENTED_EDGE ( 'NONE', *, *, #15205, .F. ) ;
#5622 = CYLINDRICAL_SURFACE ( 'NONE', #1568, 3.500000000000000000 ) ;
#5623 = ORIENTED_EDGE ( 'NONE', *, *, #16859, .F. ) ;
#5624 = AXIS2_PLACEMENT_3D ( 'NONE', #5404, #15905, #10996 ) ;
#5625 = DIRECTION ( 'NONE',  ( 0.000000000000000000, 0.000000000000000000, 1.000000000000000000 ) ) ;
#5626 = ORIENTED_EDGE ( 'NONE', *, *, #4360, .T. ) ;
#5627 = DIRECTION ( 'NONE',  ( 0.000000000000000000, 0.000000000000000000, -1.000000000000000000 ) ) ;
#5628 = ORIENTED_EDGE ( 'NONE', *, *, #12078, .F. ) ;
#5629 = AXIS2_PLACEMENT_3D ( 'NONE', #3056, #203, #15550 ) ;
#5630 = DIRECTION ( 'NONE',  ( -0.1045284632676563297, 0.9945218953682731788, 0.000000000000000000 ) ) ;
#5631 = ORIENTED_EDGE ( 'NONE', *, *, #12974, .F. ) ;
#5632 = CARTESIAN_POINT ( 'NONE',  ( 45.27934281921075410, 59.29948385550240886, -6.458785618021043895 ) ) ;
#5633 = DIRECTION ( 'NONE',  ( 0.000000000000000000, 0.000000000000000000, -1.000000000000000000 ) ) ;
#5634 = CARTESIAN_POINT ( 'NONE',  ( 46.49166364869460466, 48.69948385550241454, 4.867452303228209765 ) ) ;
#5635 = DIRECTION ( 'NONE',  ( -0.5000000000000061062, 1.060575238724902601E-16, -0.8660254037844351549 ) ) ;
#5636 = DIRECTION ( 'NONE',  ( 0.000000000000000000, -0.000000000000000000, 1.000000000000000000 ) ) ;
#5637 = CARTESIAN_POINT ( 'NONE',  ( 47.42335538002180328, 48.40051614449766504, -8.007379884777206414 ) ) ;
#5638 = AXIS2_PLACEMENT_3D ( 'NONE', #8596, #2735, #4189 ) ;
#5639 = CARTESIAN_POINT ( 'NONE',  ( 55.71335778527780036, 46.90051614449766504, -1.832500667257213056 ) ) ;
#5641 = AXIS2_PLACEMENT_3D ( 'NONE', #7161, #9800, #2582 ) ;
#5640 = CARTESIAN_POINT ( 'NONE',  ( -18.02113032590304442, -26.18033988749903074, 9.000000000000000000 ) ) ;
#5642 = VECTOR ( 'NONE', #359, 1000.000000000000000 ) ;
#5643 = DIRECTION ( 'NONE',  ( 0.3090169943749456194, 0.9510565162951541973, 0.000000000000000000 ) ) ;
#5644 = ORIENTED_EDGE ( 'NONE', *, *, #7943, .T. ) ;
#5645 = AXIS2_PLACEMENT_3D ( 'NONE', #11200, #9730, #9823 ) ;
#5646 = ORIENTED_EDGE ( 'NONE', *, *, #13098, .T. ) ;
#5647 = CARTESIAN_POINT ( 'NONE',  ( -154.9999999999999716, -14.99999999999999645, 6.499999999999999112 ) ) ;
#5648 = EDGE_LOOP ( 'NONE', ( #14542, #2614 ) ) ;
#5649 = CARTESIAN_POINT ( 'NONE',  ( 52.29715082351547295, 56.39948385550238896, 6.992620115222774047 ) ) ;
#5650 = CARTESIAN_POINT ( 'NONE',  ( 0.8816464618332836567, -24.71833652004169934, 9.999999999999998224 ) ) ;
#5651 = ORIENTED_EDGE ( 'NONE', *, *, #14442, .T. ) ;
#5652 = VERTEX_POINT ( 'NONE', #8235 ) ;
#5653 = LINE ( 'NONE', #11628, #18192 ) ;
#5654 = CIRCLE ( 'NONE', #2559, 2.649999999999985700 ) ;
#5655 = FACE_OUTER_BOUND ( 'NONE', #5723, .T. ) ;
#5656 = VERTEX_POINT ( 'NONE', #14013 ) ;
#5657 = AXIS2_PLACEMENT_3D ( 'NONE', #9679, #17548, #10074 ) ;
#5658 = CARTESIAN_POINT ( 'NONE',  ( -154.9999999999999716, -23.00000000000000000, -15.00000000000000000 ) ) ;
#5659 = VECTOR ( 'NONE', #14453, 1000.000000000000000 ) ;
#5660 = ORIENTED_EDGE ( 'NONE', *, *, #17612, .F. ) ;
#5661 = DIRECTION ( 'NONE',  ( 1.000000000000000000, 0.000000000000000000, 0.000000000000000000 ) ) ;
#5662 = CARTESIAN_POINT ( 'NONE',  ( 56.66441430157296821, 50.09948385550240602, 2.141517661632100111 ) ) ;
#5663 = DIRECTION ( 'NONE',  ( 1.000000000000000000, 0.000000000000000000, -0.000000000000000000 ) ) ;
#5664 = AXIS2_PLACEMENT_3D ( 'NONE', #16412, #9039, #7186 ) ;
#5665 = CARTESIAN_POINT ( 'NONE',  ( 56.66441430157294690, 48.90051614449766504, -2.141517661632166281 ) ) ;
#5666 = DIRECTION ( 'NONE',  ( 0.1305261922200521840, 0.9914448613738103822, 0.000000000000000000 ) ) ;
#5667 = ADVANCED_FACE ( 'NONE', ( #9420 ), #7947, .F. ) ;
#5668 = CARTESIAN_POINT ( 'NONE',  ( 0.000000000000000000, 3.755786496842903495E-16, 3.500000000000000000 ) ) ;
#5669 = EDGE_CURVE ( 'NONE', #2657, #3339, #8139, .T. ) ;
#5670 = AXIS2_PLACEMENT_3D ( 'NONE', #3043, #1572, #99 ) ;
#5671 = CIRCLE ( 'NONE', #3804, 1.000000000000000666 ) ;
#5672 = EDGE_LOOP ( 'NONE', ( #13995, #9582, #7291 ) ) ;
#5673 = ORIENTED_EDGE ( 'NONE', *, *, #17437, .T. ) ;
#5674 = DIRECTION ( 'NONE',  ( 1.000000000000000000, 0.000000000000000000, 0.000000000000000000 ) ) ;
#5675 = AXIS2_PLACEMENT_3D ( 'NONE', #10237, #12002, #16238 ) ;
#5676 = EDGE_CURVE ( 'NONE', #4769, #8689, #14417, .T. ) ;
#5677 = EDGE_CURVE ( 'NONE', #6135, #12668, #16791, .T. ) ;
#5678 = CARTESIAN_POINT ( 'NONE',  ( -54.99999999999996447, -14.99999999999998579, 15.00000000000000000 ) ) ;
#5679 =( NAMED_UNIT ( * ) PLANE_ANGLE_UNIT ( ) SI_UNIT ( $, .RADIAN. ) );
#5680 = ORIENTED_EDGE ( 'NONE', *, *, #2943, .F. ) ;
#5681 = DIRECTION ( 'NONE',  ( -1.000000000000000000, 0.000000000000000000, 0.000000000000000000 ) ) ;
#5682 = EDGE_CURVE ( 'NONE', #5258, #2819, #15308, .T. ) ;
#5683 = EDGE_CURVE ( 'NONE', #7086, #15978, #16891, .T. ) ;
#5684 = ORIENTED_EDGE ( 'NONE', *, *, #168, .F. ) ;
#5685 = ORIENTED_EDGE ( 'NONE', *, *, #4265, .T. ) ;
#5686 = DIRECTION ( 'NONE',  ( 1.000000000000000000, 0.000000000000000000, 0.000000000000000000 ) ) ;
#5687 = CIRCLE ( 'NONE', #19181, 1.000000000000001110 ) ;
#5688 = AXIS2_PLACEMENT_3D ( 'NONE', #5905, #11874, #17883 ) ;
#5689 = CARTESIAN_POINT ( 'NONE',  ( 46.49166364869456913, 50.30051614449766362, -4.867452303228181343 ) ) ;
#5690 = PLANE ( 'NONE',  #12982 ) ;
#5691 = ADVANCED_FACE ( 'NONE', ( #17663 ), #13140, .F. ) ;
#5692 = CARTESIAN_POINT ( 'NONE',  ( 4.124214193018069352, 2.028338413290941222, 3.513185186763553514 ) ) ;
#5693 = CIRCLE ( 'NONE', #10693, 12.49999999999999645 ) ;
#5694 = EDGE_CURVE ( 'NONE', #8944, #2618, #2210, .T. ) ;
#5695 = CARTESIAN_POINT ( 'NONE',  ( 56.30877334542961421, 51.99948385550239749, -0.02388180880520959434 ) ) ;
#5696 = CARTESIAN_POINT ( 'NONE',  ( 0.02993401039713615083, 3.373851915354614928, 1.156317065392238774 ) ) ;
#5697 = CARTESIAN_POINT ( 'NONE',  ( 55.96859303347804371, 52.19948385550240033, 4.306917132069425946 ) ) ;
#5698 = CARTESIAN_POINT ( 'NONE',  ( 57.61547081786810764, 48.90051614449766504, -2.450534656007114176 ) ) ;
#5699 = LINE ( 'NONE', #16392, #18485 ) ;
#5700 = VERTEX_POINT ( 'NONE', #2479 ) ;
#5701 = CARTESIAN_POINT ( 'NONE',  ( 45.60000000000000142, 0.000000000000000000, 0.000000000000000000 ) ) ;
#5702 = ADVANCED_FACE ( 'NONE', ( #11662 ), #2766, .F. ) ;
#5703 = CARTESIAN_POINT ( 'NONE',  ( -154.9999999999999716, -14.99999999999999645, 15.00000000000000000 ) ) ;
#5704 = EDGE_CURVE ( 'NONE', #10511, #468, #9514, .T. ) ;
#5705 = ORIENTED_EDGE ( 'NONE', *, *, #8789, .F. ) ;
#5706 = DIRECTION ( 'NONE',  ( 1.000000000000000000, 0.000000000000000000, 0.000000000000000000 ) ) ;
#5707 = PRODUCT_DEFINITION_SHAPE ( 'NONE', 'NONE',  #14639 ) ;
#5708 = EDGE_CURVE ( 'NONE', #6420, #1337, #10185, .T. ) ;
#5709 = AXIS2_PLACEMENT_3D ( 'NONE', #16357, #16741, #10541 ) ;
#5710 = FACE_BOUND ( 'NONE', #1454, .T. ) ;
#5711 = CARTESIAN_POINT ( 'NONE',  ( 9.999999999999994671, 20.00000000000001421, -15.00000000000000000 ) ) ;
#5712 = CARTESIAN_POINT ( 'NONE',  ( -74.99999999999997158, -22.99999999999998934, -10.00000000000000000 ) ) ;
#5713 = DIRECTION ( 'NONE',  ( 0.000000000000000000, 0.000000000000000000, -1.000000000000000000 ) ) ;
#5714 = FACE_OUTER_BOUND ( 'NONE', #3576, .T. ) ;
#5715 = CARTESIAN_POINT ( 'NONE',  ( 4.000000000000000000, -2.309401076758516691, -0.4999999999999995559 ) ) ;
#5716 = CARTESIAN_POINT ( 'NONE',  ( 42.63976443033212860, 50.99948385550240459, 0.02388180880522514787 ) ) ;
#5717 = CIRCLE ( 'NONE', #16051, 1.000000000000000000 ) ;
#5718 = DIRECTION ( 'NONE',  ( 1.000000000000000000, 0.000000000000000000, 0.000000000000000000 ) ) ;
#5719 = CARTESIAN_POINT ( 'NONE',  ( 57.61547081786812896, 50.09948385550240602, 2.450534656007040901 ) ) ;
#5720 = DIRECTION ( 'NONE',  ( 1.000000000000000000, 0.000000000000000000, 0.000000000000000000 ) ) ;
#5721 = CARTESIAN_POINT ( 'NONE',  ( 55.94051828345053679, 45.20051614449764088, 4.345558710429044069 ) ) ;
#5722 = DIRECTION ( 'NONE',  ( 0.000000000000000000, 0.000000000000000000, -1.000000000000000000 ) ) ;
#5723 = EDGE_LOOP ( 'NONE', ( #14570, #18536, #6745, #15319 ) ) ;
#5724 = ORIENTED_EDGE ( 'NONE', *, *, #644, .T. ) ;
#5725 = CARTESIAN_POINT ( 'NONE',  ( 8.500000000000000000, 2.886751345948123770, -5.000000000000000000 ) ) ;
#5726 = ORIENTED_EDGE ( 'NONE', *, *, #3071, .F. ) ;
#5727 = DIRECTION ( 'NONE',  ( 1.000000000000000000, 0.000000000000000000, -0.000000000000000000 ) ) ;
#5728 = VERTEX_POINT ( 'NONE', #12942 ) ;
#5729 = CARTESIAN_POINT ( 'NONE',  ( 2.449293598294706513E-15, -20.00000000000000000, 9.000000000000000000 ) ) ;
#5730 = ADVANCED_FACE ( 'NONE', ( #16091 ), #8725, .F. ) ;
#5731 = EDGE_LOOP ( 'NONE', ( #9192, #310, #9849, #3672 ) ) ;
#5732 = CYLINDRICAL_SURFACE ( 'NONE', #15564, 2.649999999999985700 ) ;
#5733 = VERTEX_POINT ( 'NONE', #17478 ) ;
#5734 = VERTEX_POINT ( 'NONE', #16185 ) ;
#5735 = CARTESIAN_POINT ( 'NONE',  ( 47.42335538002188144, 60.59948385550240602, 8.007379884777233059 ) ) ;
#5736 = FACE_OUTER_BOUND ( 'NONE', #7293, .T. ) ;
#5737 = EDGE_CURVE ( 'NONE', #10144, #10530, #8431, .T. ) ;
#5738 = CARTESIAN_POINT ( 'NONE',  ( 53.50833635130540955, 51.69948385550241454, -4.867452303228209765 ) ) ;
#5739 = LINE ( 'NONE', #9840, #8846 ) ;
#5740 = DIRECTION ( 'NONE',  ( 0.000000000000000000, -1.000000000000000000, 0.000000000000000000 ) ) ;
#5741 = CARTESIAN_POINT ( 'NONE',  ( 41.58830220609386430, 50.00051614449765935, -0.02388180880514929535 ) ) ;
#5742 = CARTESIAN_POINT ( 'NONE',  ( 49.97728705011494554, 51.50051614449765935, 6.000000000000000888 ) ) ;
#5743 = DIRECTION ( 'NONE',  ( 0.000000000000000000, 0.000000000000000000, 1.000000000000000000 ) ) ;
#5744 = CARTESIAN_POINT ( 'NONE',  ( 1.567478505476134606E-15, 4.618802153517012066, -3.433295621305382905 ) ) ;
#5745 = ORIENTED_EDGE ( 'NONE', *, *, #8716, .T. ) ;
#5746 = ORIENTED_EDGE ( 'NONE', *, *, #4625, .T. ) ;
#5747 = DIRECTION ( 'NONE',  ( 0.000000000000000000, 0.000000000000000000, 1.000000000000000000 ) ) ;
#5748 = ORIENTED_EDGE ( 'NONE', *, *, #748, .F. ) ;
#5749 = CARTESIAN_POINT ( 'NONE',  ( 0.000000000000000000, 4.330127018922190096, -2.500000000000006217 ) ) ;
#5750 = DIRECTION ( 'NONE',  ( -9.858538378746663627E-23, 5.031452844637890958E-23, -1.000000000000000000 ) ) ;
#5751 = ORIENTED_EDGE ( 'NONE', *, *, #7832, .F. ) ;
#5752 = ORIENTED_EDGE ( 'NONE', *, *, #8061, .T. ) ;
#5753 = FACE_OUTER_BOUND ( 'NONE', #13702, .T. ) ;
#5754 = DIRECTION ( 'NONE',  ( -1.000000000000000000, 0.000000000000000000, 0.000000000000000000 ) ) ;
#5755 = AXIS2_PLACEMENT_3D ( 'NONE', #17515, #17707, #9938 ) ;
#5756 = EDGE_LOOP ( 'NONE', ( #14976, #4476, #17749, #4016, #12995 ) ) ;
#5757 = FACE_OUTER_BOUND ( 'NONE', #803, .T. ) ;
#5758 = ORIENTED_EDGE ( 'NONE', *, *, #11309, .F. ) ;
#5759 = AXIS2_PLACEMENT_3D ( 'NONE', #8457, #11684, #7279 ) ;
#5760 = DIRECTION ( 'NONE',  ( -0.000000000000000000, -0.000000000000000000, 1.000000000000000000 ) ) ;
#5761 = CARTESIAN_POINT ( 'NONE',  ( 45.86712807150323812, 49.29948385550240175, -5.649768623646098220 ) ) ;
#5762 = LINE ( 'NONE', #11533, #532 ) ;
#5763 = CARTESIAN_POINT ( 'NONE',  ( 55.94051828345053679, 45.20051614449764088, 4.345558710429044069 ) ) ;
#5764 = CARTESIAN_POINT ( 'NONE',  ( -9.999999999999998224, 15.00000000000001776, 15.00000000000000000 ) ) ;
#5765 = DIRECTION ( 'NONE',  ( -0.000000000000000000, -0.000000000000000000, 1.000000000000000000 ) ) ;
#5766 = DIRECTION ( 'NONE',  ( 0.8090169943749546677, -0.5877852522924632561, 0.000000000000000000 ) ) ;
#5767 = VECTOR ( 'NONE', #8481, 1000.000000000000000 ) ;
#5768 = ORIENTED_EDGE ( 'NONE', *, *, #8194, .T. ) ;
#5769 = EDGE_LOOP ( 'NONE', ( #1828, #8505, #1516, #11021, #16379, #9093 ) ) ;
#5770 = CARTESIAN_POINT ( 'NONE',  ( 1.566204647097437341, -6.822536405429464601, 0.000000000000000000 ) ) ;
#5771 = FILL_AREA_STYLE ('',( #8809 ) ) ;
#5772 = CIRCLE ( 'NONE', #6374, 8.000000000000000000 ) ;
#5773 = CYLINDRICAL_SURFACE ( 'NONE', #241, 2.649999999999985700 ) ;
#5774 = B_SPLINE_CURVE_WITH_KNOTS ( 'NONE', 3,
 ( #16956, #565, #9476, #6441, #17144, #3605 ),
 .UNSPECIFIED., .F., .F.,
 ( 4, 2, 4 ),
 ( 0.002044882221487524104, 0.003063384235218490244, 0.004081886248949456383 ),
 .UNSPECIFIED. ) ;
#5775 = DIRECTION ( 'NONE',  ( -1.000000000000000000, -1.040834085586084257E-16, -0.000000000000000000 ) ) ;
#5776 = ORIENTED_EDGE ( 'NONE', *, *, #12870, .F. ) ;
#5777 = CARTESIAN_POINT ( 'NONE',  ( -54.99999999999996447, -14.99999999999998579, -10.00000000000000178 ) ) ;
#5778 = EDGE_CURVE ( 'NONE', #16922, #16847, #2263, .T. ) ;
#5779 = ORIENTED_EDGE ( 'NONE', *, *, #4959, .F. ) ;
#5780 = EDGE_LOOP ( 'NONE', ( #657, #1824 ) ) ;
#5781 = CARTESIAN_POINT ( 'NONE',  ( -1.150000000000001688, 0.000000000000000000, 0.000000000000000000 ) ) ;
#5782 = UNCERTAINTY_MEASURE_WITH_UNIT (LENGTH_MEASURE( 1.000000000000000082E-05 ), #1835, 'distance_accuracy_value', 'NONE');
#5783 = CARTESIAN_POINT ( 'NONE',  ( -74.99999999999997158, -39.99999999999998579, -20.00000000000000000 ) ) ;
#5784 = AXIS2_PLACEMENT_3D ( 'NONE', #2971, #7659, #11975 ) ;
#5785 = CARTESIAN_POINT ( 'NONE',  ( 55.11794222512599362, 48.80051614449767072, -3.688883143319583446 ) ) ;
#5786 = FACE_OUTER_BOUND ( 'NONE', #15131, .T. ) ;
#5787 = CARTESIAN_POINT ( 'NONE',  ( 49.97728705011488870, 57.49948385550241170, -6.000000000000000888 ) ) ;
#5788 = LINE ( 'NONE', #1578, #19135 ) ;
#5789 = CARTESIAN_POINT ( 'NONE',  ( 45.86712807150323812, 51.29948385550240175, -5.649768623646098220 ) ) ;
#5790 = CARTESIAN_POINT ( 'NONE',  ( 41.58830220609386430, 50.00051614449765935, -0.02388180880514929535 ) ) ;
#5791 = CARTESIAN_POINT ( 'NONE',  ( -4.113721387458914807E-15, -4.207632145829740544, 2.712167343862823099 ) ) ;
#5792 = EDGE_CURVE ( 'NONE', #965, #16399, #6963, .T. ) ;
#5793 = CARTESIAN_POINT ( 'NONE',  ( 2.000000000000000000, -0.8865213383406694847, 1.535500000000001419 ) ) ;
#5794 = PRODUCT_CONTEXT ( 'NONE', #8877, 'mechanical' ) ;
#5795 = VECTOR ( 'NONE', #16551, 1000.000000000000000 ) ;
#5796 = ORIENTED_EDGE ( 'NONE', *, *, #12047, .T. ) ;
#5797 = CIRCLE ( 'NONE', #7347, 1.000000000000001110 ) ;
#5798 = DIRECTION ( 'NONE',  ( -0.000000000000000000, -0.000000000000000000, -1.000000000000000000 ) ) ;
#5799 = EDGE_CURVE ( 'NONE', #18786, #11939, #14600, .T. ) ;
#5800 = EDGE_CURVE ( 'NONE', #3297, #4766, #17954, .T. ) ;
#5801 = CARTESIAN_POINT ( 'NONE',  ( -74.99999999999997158, 45.00000000000001421, 15.00000000000000000 ) ) ;
#5802 = EDGE_CURVE ( 'NONE', #17702, #13670, #18748, .T. ) ;
#5803 = CARTESIAN_POINT ( 'NONE',  ( -62.49999999999997158, 32.50000000000001421, 15.00000000000000000 ) ) ;
#5804 = DIRECTION ( 'NONE',  ( 0.000000000000000000, 0.000000000000000000, 1.000000000000000000 ) ) ;
#5805 = CARTESIAN_POINT ( 'NONE',  ( 6.533910050139694725, 2.950514251728050485, 5.110440592449069896 ) ) ;
#5806 = DIRECTION ( 'NONE',  ( 1.000000000000000000, 0.000000000000000000, 0.000000000000000000 ) ) ;
#5807 = EDGE_CURVE ( 'NONE', #17921, #16520, #14505, .T. ) ;
#5808 = CARTESIAN_POINT ( 'NONE',  ( 0.1085714285714285687, -3.798448662927795372, -0.8000000000000000444 ) ) ;
#5809 = CARTESIAN_POINT ( 'NONE',  ( 45.90387839640214196, 50.69948385550240744, 5.676469297603166098 ) ) ;
#5810 = DIRECTION ( 'NONE',  ( -0.000000000000000000, -0.000000000000000000, 1.000000000000000000 ) ) ;
#5811 = CARTESIAN_POINT ( 'NONE',  ( 47.42335538002188144, 54.59948385550240602, 8.007379884777233059 ) ) ;
#5812 = DIRECTION ( 'NONE',  ( 0.000000000000000000, 0.8660254037844380415, -0.5000000000000012212 ) ) ;
#5813 = CARTESIAN_POINT ( 'NONE',  ( 50.02271294988505446, 50.50051614449765935, -7.000000000000000888 ) ) ;
#5814 = LINE ( 'NONE', #16316, #2554 ) ;
#5815 = CIRCLE ( 'NONE', #10194, 0.9999999999999982236 ) ;
#5816 = VERTEX_POINT ( 'NONE', #15796 ) ;
#5817 = VERTEX_POINT ( 'NONE', #2377 ) ;
#5818 = FACE_OUTER_BOUND ( 'NONE', #5267, .T. ) ;
#5819 = ORIENTED_EDGE ( 'NONE', *, *, #3055, .F. ) ;
#5820 = EDGE_CURVE ( 'NONE', #13173, #8527, #15709, .T. ) ;
#5821 = VECTOR ( 'NONE', #6063, 1000.000000000000000 ) ;
#5822 = EDGE_CURVE ( 'NONE', #439, #8857, #18238, .T. ) ;
#5823 = DIRECTION ( 'NONE',  ( 1.000000000000000000, 0.000000000000000000, 0.000000000000000000 ) ) ;
#5824 = ORIENTED_EDGE ( 'NONE', *, *, #17008, .T. ) ;
#5825 = DIRECTION ( 'NONE',  ( 1.000000000000000000, 0.000000000000000000, 0.000000000000000000 ) ) ;
#5826 = VERTEX_POINT ( 'NONE', #9994 ) ;
#5827 = CARTESIAN_POINT ( 'NONE',  ( -2.688821387764050996E-14, -4.618802153517012954, -0.4999999999999995559 ) ) ;
#5828 = ORIENTED_EDGE ( 'NONE', *, *, #5682, .T. ) ;
#5829 = CARTESIAN_POINT ( 'NONE',  ( 47.37792948025162332, 61.39948385550240317, -7.992620115222770494 ) ) ;
#5830 = CARTESIAN_POINT ( 'NONE',  ( -59.84999999999998721, 32.50000000000001421, 15.00000000000000000 ) ) ;
#5831 = AXIS2_PLACEMENT_3D ( 'NONE', #11432, #11338, #4094 ) ;
#5832 = CARTESIAN_POINT ( 'NONE',  ( 48.02776887271745210, 59.39948385550240317, -5.992620115222778487 ) ) ;
#5833 = DIRECTION ( 'NONE',  ( 0.000000000000000000, 0.000000000000000000, -1.000000000000000000 ) ) ;
#5834 = CARTESIAN_POINT ( 'NONE',  ( -32.00000000000000000, 1.000000000000000000, -5.999999999999998224 ) ) ;
#5835 = CARTESIAN_POINT ( 'NONE',  ( 52.57664461997821093, 53.40051614449765793, 8.007379884777206414 ) ) ;
#5836 = CARTESIAN_POINT ( 'NONE',  ( 44.88205777487401349, 47.80051614449764941, 3.688883143319584779 ) ) ;
#5837 = CIRCLE ( 'NONE', #205, 4.872650870659752442 ) ;
#5838 = DIRECTION ( 'NONE',  ( 0.000000000000000000, 0.000000000000000000, -1.000000000000000000 ) ) ;
#5839 = CARTESIAN_POINT ( 'NONE',  ( 5.599999999999999645, 4.041451884327382338, 0.000000000000000000 ) ) ;
#5840 = ORIENTED_EDGE ( 'NONE', *, *, #1780, .F. ) ;
#5841 = ORIENTED_EDGE ( 'NONE', *, *, #15145, .F. ) ;
#5842 = CARTESIAN_POINT ( 'NONE',  ( 18.68843350152485527, -12.87662627267923909, 0.000000000000000000 ) ) ;
#5843 = VECTOR ( 'NONE', #18673, 1000.000000000000000 ) ;
#5844 = ORIENTED_EDGE ( 'NONE', *, *, #18887, .T. ) ;
#5845 = ADVANCED_FACE ( 'NONE', ( #5592 ), #7299, .F. ) ;
#5846 = CARTESIAN_POINT ( 'NONE',  ( 43.34962307344081012, 64.89948385550239607, 2.184720259617164650 ) ) ;
#5847 = CARTESIAN_POINT ( 'NONE',  ( 50.02271294988505446, 64.50051614449765225, -7.000000000000000888 ) ) ;
#5848 = EDGE_CURVE ( 'NONE', #2897, #6112, #7643, .T. ) ;
#5849 = ORIENTED_EDGE ( 'NONE', *, *, #12619, .T. ) ;
#5850 = LINE ( 'NONE', #1440, #4717 ) ;
#5851 = CARTESIAN_POINT ( 'NONE',  ( 55.96859303347805081, 48.19948385550240744, 4.306917132069425058 ) ) ;
#5852 = EDGE_CURVE ( 'NONE', #3997, #6513, #5788, .T. ) ;
#5853 = ORIENTED_EDGE ( 'NONE', *, *, #2466, .F. ) ;
#5854 = CARTESIAN_POINT ( 'NONE',  ( 2.449293598294706513E-15, -20.00000000000000000, -50.00000000000000000 ) ) ;
#5855 = ORIENTED_EDGE ( 'NONE', *, *, #14806, .T. ) ;
#5856 = DIRECTION ( 'NONE',  ( -1.000000000000000000, 0.000000000000000000, 0.000000000000000000 ) ) ;
#5857 = AXIS2_PLACEMENT_3D ( 'NONE', #11501, #17614, #14635 ) ;
#5858 = CARTESIAN_POINT ( 'NONE',  ( 57.36023556966787851, 57.99948385550239038, -0.02388180880522424582 ) ) ;
#5859 = CARTESIAN_POINT ( 'NONE',  ( -14.17539641854921229, -5.891203581560112923, -9.000000000000000000 ) ) ;
#5860 = CIRCLE ( 'NONE', #12736, 7.500000000000000888 ) ;
#5861 = CARTESIAN_POINT ( 'NONE',  ( 43.33558569842706021, 45.90051614449765793, 2.141517661632167169 ) ) ;
#5862 = CARTESIAN_POINT ( 'NONE',  ( 7.336184427528458230, 0.000000000000000000, 0.000000000000000000 ) ) ;
#5863 = CARTESIAN_POINT ( 'NONE',  ( -4.000000000000000000, 0.8576368993457507139, -3.433240632782198709 ) ) ;
#5864 = EDGE_LOOP ( 'NONE', ( #9344, #6932, #10169, #7931 ) ) ;
#5865 = EDGE_CURVE ( 'NONE', #6937, #4747, #12261, .T. ) ;
#5866 = CLOSED_SHELL ( 'NONE', ( #19264, #12279, #18324, #11424, #7297, #14652, #9924, #9749, #15801, #876, #9900, #4614, #18642, #11325, #6067, #8324, #8547, #15027, #6184, #3880 ) ) ;
#5867 = PRODUCT_DEFINITION_SHAPE ( 'NONE', 'NONE',  #19419 ) ;
#5868 = ORIENTED_EDGE ( 'NONE', *, *, #1392, .T. ) ;
#5869 = ORIENTED_EDGE ( 'NONE', *, *, #15919, .F. ) ;
#5870 = DIRECTION ( 'NONE',  ( 1.000000000000000000, 0.000000000000000000, 0.000000000000000000 ) ) ;
#5871 = ADVANCED_FACE ( 'NONE', ( #9012 ), #16389, .T. ) ;
#5872 = AXIS2_PLACEMENT_3D ( 'NONE', #16173, #9977, #14585 ) ;
#5873 = CARTESIAN_POINT ( 'NONE',  ( 42.38452918213188525, 65.09948385550239891, -2.450534656007040013 ) ) ;
#5874 = CARTESIAN_POINT ( 'NONE',  ( 0.000000000000000000, 0.000000000000000000, 0.000000000000000000 ) ) ;
#5875 = EDGE_LOOP ( 'NONE', ( #114, #3822, #11936, #6807 ) ) ;
#5876 = AXIS2_PLACEMENT_3D ( 'NONE', #3686, #9651, #15646 ) ;
#5877 = CARTESIAN_POINT ( 'NONE',  ( -4.211140560182196957, -2.431303136016552013, -3.745885042887436178 ) ) ;
#5878 = VERTEX_POINT ( 'NONE', #6085 ) ;
#5879 = VERTEX_POINT ( 'NONE', #16290 ) ;
#5880 = DIRECTION ( 'NONE',  ( 0.000000000000000000, 0.000000000000000000, -1.000000000000000000 ) ) ;
#5881 = DIRECTION ( 'NONE',  ( -9.858538378746663627E-23, 5.031452844637890958E-23, -1.000000000000000000 ) ) ;
#5882 = AXIS2_PLACEMENT_3D ( 'NONE', #13913, #9317, #3545 ) ;
#5883 = CARTESIAN_POINT ( 'NONE',  ( 46.45491332379576477, 45.70051614449766220, 4.840751629271188961 ) ) ;
#5884 = PLANE ( 'NONE',  #10782 ) ;
#5885 = DIRECTION ( 'NONE',  ( 0.000000000000000000, -0.000000000000000000, 1.000000000000000000 ) ) ;
#5886 = CARTESIAN_POINT ( 'NONE',  ( 46.45491332379572924, 57.29948385550240175, -4.840751629271157874 ) ) ;
#5887 = CARTESIAN_POINT ( 'NONE',  ( 0.6640947660595348800, -4.471078309994175548, -3.602146406945708090 ) ) ;
#5888 = AXIS2_PLACEMENT_3D ( 'NONE', #3978, #2907, #11612 ) ;
#5889 = CARTESIAN_POINT ( 'NONE',  ( 55.94051828345050836, 55.79948385550238044, -4.345558710429104465 ) ) ;
#5890 = CARTESIAN_POINT ( 'NONE',  ( 52.62207051974829852, 56.60051614449765367, -7.992620115222797139 ) ) ;
#5891 = LINE ( 'NONE', #2585, #16912 ) ;
#5892 = CARTESIAN_POINT ( 'NONE',  ( 3.951447005078450925, -2.357513599190971032, 2.916666666666666963 ) ) ;
#5893 = CARTESIAN_POINT ( 'NONE',  ( 2.449293598294706513E-15, -20.00000000000000000, 9.000000000000000000 ) ) ;
#5894 =( LENGTH_UNIT ( ) NAMED_UNIT ( * ) SI_UNIT ( .MILLI., .METRE. ) );
#5895 = ORIENTED_EDGE ( 'NONE', *, *, #12720, .T. ) ;
#5896 = CARTESIAN_POINT ( 'NONE',  ( -3.540020015735593439, -2.810662092924100630, -3.602146406945814672 ) ) ;
#5897 =( GEOMETRIC_REPRESENTATION_CONTEXT ( 3 ) GLOBAL_UNCERTAINTY_ASSIGNED_CONTEXT ( ( #4802 ) ) GLOBAL_UNIT_ASSIGNED_CONTEXT ( ( #11254, #5679, #5386 ) ) REPRESENTATION_CONTEXT ( 'NONE', 'WORKASPACE' ) );
#5898 = CARTESIAN_POINT ( 'NONE',  ( 2.449293598294706513E-15, -20.00000000000000000, 9.000000000000000000 ) ) ;
#5899 = DIRECTION ( 'NONE',  ( -0.000000000000000000, -0.000000000000000000, 1.000000000000000000 ) ) ;
#5900 = DIRECTION ( 'NONE',  ( 1.000000000000000000, 0.000000000000000000, 0.000000000000000000 ) ) ;
#5901 = FACE_OUTER_BOUND ( 'NONE', #18988, .T. ) ;
#5902 = DIRECTION ( 'NONE',  ( 0.000000000000000000, 0.000000000000000000, 1.000000000000000000 ) ) ;
#5903 = DIRECTION ( 'NONE',  ( 0.000000000000000000, 0.000000000000000000, -1.000000000000000000 ) ) ;
#5904 = CARTESIAN_POINT ( 'NONE',  ( 44.03140696652192787, 59.19948385550238612, -4.306917132069425058 ) ) ;
#5905 = CARTESIAN_POINT ( 'NONE',  ( 2.449293598294706513E-15, -20.00000000000000000, 15.00000000000000355 ) ) ;
#5906 = CARTESIAN_POINT ( 'NONE',  ( 52.57664461997811856, 53.59948385550240602, -8.007379884777229506 ) ) ;
#5907 = CARTESIAN_POINT ( 'NONE',  ( 0.000000000000000000, 0.000000000000000000, 0.000000000000000000 ) ) ;
#5908 = CONICAL_SURFACE ( 'NONE', #13116, 1.999999999999998224, 1.029744259999999745 ) ;
#5909 = EDGE_CURVE ( 'NONE', #8263, #1014, #8138, .T. ) ;
#5910 = CARTESIAN_POINT ( 'NONE',  ( 50.02271294988505446, 54.50051614449765935, -7.000000000000000888 ) ) ;
#5911 = VECTOR ( 'NONE', #17338, 1000.000000000000000 ) ;
#5912 = CARTESIAN_POINT ( 'NONE',  ( -1.249999999999997558, 0.000000000000000000, 0.000000000000000000 ) ) ;
#5913 = ORIENTED_EDGE ( 'NONE', *, *, #13110, .F. ) ;
#5914 = ADVANCED_FACE ( 'NONE', ( #10388 ), #2954, .F. ) ;
#5915 =( GEOMETRIC_REPRESENTATION_CONTEXT ( 3 ) GLOBAL_UNCERTAINTY_ASSIGNED_CONTEXT ( ( #12427 ) ) GLOBAL_UNIT_ASSIGNED_CONTEXT ( ( #15851, #18812, #16948 ) ) REPRESENTATION_CONTEXT ( 'NONE', 'WORKASPACE' ) );
#5916 = ORIENTED_EDGE ( 'NONE', *, *, #3582, .F. ) ;
#5917 = CARTESIAN_POINT ( 'NONE',  ( 2.000000000000000000, -1.773042676681341856, 2.276824562219559311E-15 ) ) ;
#5918 = EDGE_LOOP ( 'NONE', ( #15127, #17041, #7317 ) ) ;
#5919 = EDGE_CURVE ( 'NONE', #7980, #628, #13535, .T. ) ;
#5920 = ADVANCED_FACE ( 'NONE', ( #107 ), #5995, .F. ) ;
#5921 = FACE_OUTER_BOUND ( 'NONE', #11880, .T. ) ;
#5922 = ADVANCED_BREP_SHAPE_REPRESENTATION ( '', ( #15206, #10359 ), #13801 ) ;
#5923 = ORIENTED_EDGE ( 'NONE', *, *, #17326, .F. ) ;
#5924 = CARTESIAN_POINT ( 'NONE',  ( 62.49999999999998579, 40.00000000000001421, -9.999999999999998224 ) ) ;
#5925 = AXIS2_PLACEMENT_3D ( 'NONE', #853, #2249, #5547 ) ;
#5926 = CIRCLE ( 'NONE', #4051, 20.00000000000000000 ) ;
#5927 = EDGE_CURVE ( 'NONE', #7385, #8711, #4423, .T. ) ;
#5928 = ORIENTED_EDGE ( 'NONE', *, *, #4733, .F. ) ;
#5929 = CARTESIAN_POINT ( 'NONE',  ( 50.00000000000000000, 40.00000000000000000, 0.000000000000000000 ) ) ;
#5930 = ORIENTED_EDGE ( 'NONE', *, *, #11172, .T. ) ;
#5931 =( BOUNDED_SURFACE ( )  B_SPLINE_SURFACE ( 3, 2, ( 
 ( #14571, #15695, #4193 ),
 ( #5190, #2739, #17540 ),
 ( #11634, #13109, #7229 ),
 ( #8696, #4389, #9695 ),
 ( #17643, #10255, #19317 ),
 ( #17170, #2276, #14670 ) ),
 .UNSPECIFIED., .F., .F., .T. ) 
 B_SPLINE_SURFACE_WITH_KNOTS ( ( 4, 2, 4 ),
 ( 3, 3 ),
 ( 0.02032853247518125531, 0.02278863295364820865, 0.02524873343211516200 ),
 ( 0.000000000000000000, 1.000000000000000000 ),
 .UNSPECIFIED. ) 
 GEOMETRIC_REPRESENTATION_ITEM ( )  RATIONAL_B_SPLINE_SURFACE ( (
 ( 1.000000000000000000, 0.8047781615896836271, 1.000000000000000000),
 ( 1.000000000000000000, 0.8123767586289967202, 1.000000000000000000),
 ( 1.000000000000000000, 0.8190662415563443322, 1.000000000000000000),
 ( 1.000000000000000000, 0.8192361015669982205, 1.000000000000000000),
 ( 1.000000000000000000, 0.8126135807103181952, 1.000000000000000000),
 ( 1.000000000000000000, 0.8047712338318587788, 1.000000000000000000) ) ) 
 REPRESENTATION_ITEM ( '' )  SURFACE ( )  );
#5932 = DIRECTION ( 'NONE',  ( 0.1305261922200521840, 0.9914448613738103822, -0.000000000000000000 ) ) ;
#5933 = CARTESIAN_POINT ( 'NONE',  ( 75.00000000000002842, -2.999999999999999112, 6.000000000000003553 ) ) ;
#5934 = CARTESIAN_POINT ( 'NONE',  ( 53.54508667620428497, 56.29948385550240886, 4.840751629271157874 ) ) ;
#5935 = DIRECTION ( 'NONE',  ( 0.000000000000000000, 0.000000000000000000, -1.000000000000000000 ) ) ;
#5936 = CARTESIAN_POINT ( 'NONE',  ( 47.37792948025170858, 55.60051614449765367, 7.992620115222797139 ) ) ;
#5937 = EDGE_CURVE ( 'NONE', #16193, #15389, #15991, .T. ) ;
#5938 = CARTESIAN_POINT ( 'NONE',  ( 55.08986747509849380, 49.20051614449766220, 3.727524721679155384 ) ) ;
#5939 = EDGE_CURVE ( 'NONE', #6090, #7143, #16579, .T. ) ;
#5940 = CARTESIAN_POINT ( 'NONE',  ( 32.49999999999998579, 45.00000000000001421, 5.000000000000003553 ) ) ;
#5941 = CARTESIAN_POINT ( 'NONE',  ( 4.158233816355333623, -39.56295201467608535, -9.000000000000000000 ) ) ;
#5942 = AXIS2_PLACEMENT_3D ( 'NONE', #19083, #1413, #19383 ) ;
#5943 = VERTEX_POINT ( 'NONE', #10676 ) ;
#5944 = VECTOR ( 'NONE', #309, 1000.000000000000000 ) ;
#5945 = ORIENTED_EDGE ( 'NONE', *, *, #591, .T. ) ;
#5946 = LINE ( 'NONE', #7117, #4038 ) ;
#5947 = ORIENTED_EDGE ( 'NONE', *, *, #7232, .T. ) ;
#5948 = CARTESIAN_POINT ( 'NONE',  ( -155.0818120241833640, -18.99916326157099178, 17.00000000000000000 ) ) ;
#5949 = DIRECTION ( 'NONE',  ( 0.000000000000000000, 0.000000000000000000, 1.000000000000000000 ) ) ;
#5950 = CIRCLE ( 'NONE', #10621, 2.649999999999985700 ) ;
#5951 = ORIENTED_EDGE ( 'NONE', *, *, #18214, .T. ) ;
#5952 = CARTESIAN_POINT ( 'NONE',  ( 75.00000000000001421, -7.499999999999971578, -20.00000000000000000 ) ) ;
#5953 = CARTESIAN_POINT ( 'NONE',  ( 0.1374368770859597522, -4.808326913195983821, -0.8000000000000000444 ) ) ;
#5954 = EDGE_LOOP ( 'NONE', ( #16878, #157 ) ) ;
#5955 = DIRECTION ( 'NONE',  ( -0.000000000000000000, -0.000000000000000000, 1.000000000000000000 ) ) ;
#5956 = ORIENTED_EDGE ( 'NONE', *, *, #16411, .F. ) ;
#5957 = CARTESIAN_POINT ( 'NONE',  ( 58.41169779390614281, 63.00051614449766646, 0.02388180880515032231 ) ) ;
#5958 = VECTOR ( 'NONE', #16196, 1000.000000000000000 ) ;
#5959 = DIRECTION ( 'NONE',  ( 0.000000000000000000, 1.000000000000000000, 0.000000000000000000 ) ) ;
#5960 = CARTESIAN_POINT ( 'NONE',  ( 54.13287192849676188, 60.29948385550240886, 5.649768623646098220 ) ) ;
#5961 = CARTESIAN_POINT ( 'NONE',  ( -4.158233816355060064, -39.56295201467614220, -9.000000000000000000 ) ) ;
#5962 = DIRECTION ( 'NONE',  ( 0.000000000000000000, 0.000000000000000000, 1.000000000000000000 ) ) ;
#5963 = CARTESIAN_POINT ( 'NONE',  ( 44.03140696652198471, 53.80051614449766362, 4.306917132069485454 ) ) ;
#5964 = CARTESIAN_POINT ( 'NONE',  ( -158.7998746980210001, -15.03085902363206472, 15.00000000000000000 ) ) ;
#5965 = PLANE ( 'NONE',  #13947 ) ;
#5966 = AXIS2_PLACEMENT_3D ( 'NONE', #11810, #1635, #17814 ) ;
#5967 = B_SPLINE_CURVE_WITH_KNOTS ( 'NONE', 3,
 ( #11380, #1304, #16198, #7273, #2969, #6975, #13152, #14613 ),
 .UNSPECIFIED., .F., .F.,
 ( 4, 2, 2, 4 ),
 ( 0.000000000000000000, 0.002450665683189820997, 0.003675998524784731495, 0.004901331366379641993 ),
 .UNSPECIFIED. ) ;
#5968 = FACE_OUTER_BOUND ( 'NONE', #5971, .T. ) ;
#5969 = EDGE_LOOP ( 'NONE', ( #10642, #11814, #14582, #17945 ) ) ;
#5970 = VERTEX_POINT ( 'NONE', #11752 ) ;
#5971 = EDGE_LOOP ( 'NONE', ( #10212, #6988, #5431, #1851 ) ) ;
#5972 = LINE ( 'NONE', #7145, #16867 ) ;
#5973 = SURFACE_STYLE_USAGE ( .BOTH. , #4112 ) ;
#5974 = CARTESIAN_POINT ( 'NONE',  ( 50.02271294988513972, 64.49948385550239038, 8.000000000000001776 ) ) ;
#5975 = CARTESIAN_POINT ( 'NONE',  ( 14.14213562373094923, -14.99999999999999112, -50.00000000000000000 ) ) ;
#5976 = AXIS2_PLACEMENT_3D ( 'NONE', #13897, #9206, #2154 ) ;
#5977 = AXIS2_PLACEMENT_3D ( 'NONE', #13675, #1644, #13583 ) ;
#5978 = EDGE_LOOP ( 'NONE', ( #14095, #13335, #8853, #6829 ) ) ;
#5979 = CARTESIAN_POINT ( 'NONE',  ( 6.534224484704327374, 5.901860969583204941, 2.029550679094937724E-14 ) ) ;
#5980 = VECTOR ( 'NONE', #13355, 1000.000000000000000 ) ;
#5981 = ORIENTED_EDGE ( 'NONE', *, *, #1262, .F. ) ;
#5982 = CARTESIAN_POINT ( 'NONE',  ( 54.13287192849671214, 60.70051614449766220, -5.649768623646139964 ) ) ;
#5983 = ORIENTED_EDGE ( 'NONE', *, *, #11667, .F. ) ;
#5984 = EDGE_CURVE ( 'NONE', #2487, #7000, #17877, .T. ) ;
#5985 = LINE ( 'NONE', #1861, #17586 ) ;
#5986 = UNCERTAINTY_MEASURE_WITH_UNIT (LENGTH_MEASURE( 1.000000000000000082E-05 ), #5282, 'distance_accuracy_value', 'NONE');
#5987 = CARTESIAN_POINT ( 'NONE',  ( 0.1388410611046082266, -2.351840044243035166, 2.926493552096024242 ) ) ;
#5989 = AXIS2_PLACEMENT_3D ( 'NONE', #19040, #19143, #5686 ) ;
#5988 = CARTESIAN_POINT ( 'NONE',  ( 55.69932041026405045, 55.10051614449765367, 1.875703265242156359 ) ) ;
#5990 = PLANE ( 'NONE',  #13909 ) ;
#5991 = EDGE_CURVE ( 'NONE', #585, #6953, #13484, .T. ) ;
#5992 = CARTESIAN_POINT ( 'NONE',  ( -19.89043790736545603, -22.09056926535314602, -9.000000000000000000 ) ) ;
#5993 = CARTESIAN_POINT ( 'NONE',  ( 51.92680522751233951, 55.59948385550240602, -6.007379884777223289 ) ) ;
#5994 = AXIS2_PLACEMENT_3D ( 'NONE', #1554, #1264, #7431 ) ;
#5995 = CYLINDRICAL_SURFACE ( 'NONE', #17246, 4.000000000000003553 ) ;
#5996 = CIRCLE ( 'NONE', #39, 0.4999999999999972244 ) ;
#5997 = CARTESIAN_POINT ( 'NONE',  ( 49.97728705011488159, 51.49948385550240459, -7.000000000000000888 ) ) ;
#5998 = VECTOR ( 'NONE', #19401, 1000.000000000000000 ) ;
#5999 = CARTESIAN_POINT ( 'NONE',  ( 56.79116909180259398, 53.20051614449766220, 4.963592699178938972 ) ) ;
#6000 = CARTESIAN_POINT ( 'NONE',  ( 6.390983399715589819, -2.822795037344614233, 5.110775575965824657 ) ) ;
#6001 = CARTESIAN_POINT ( 'NONE',  ( 4.158921614371307030, 1.986121848748763741, -3.559936047944503912 ) ) ;
#6002 = ORIENTED_EDGE ( 'NONE', *, *, #17573, .T. ) ;
#6003 = CARTESIAN_POINT ( 'NONE',  ( 7.211304515372431112, -1.345319965580505484, -9.000000000000000000 ) ) ;
#6004 = PRESENTATION_STYLE_ASSIGNMENT (( #15 ) ) ;
#6005 = DIRECTION ( 'NONE',  ( 1.000000000000000000, 0.000000000000000000, 0.000000000000000000 ) ) ;
#6006 = ORIENTED_EDGE ( 'NONE', *, *, #6879, .F. ) ;
#6007 = DIRECTION ( 'NONE',  ( 1.000000000000000000, 0.000000000000000000, 0.000000000000000000 ) ) ;
#6008 = CARTESIAN_POINT ( 'NONE',  ( 4.050536630291688311, 2.401306687817038821, -2.976670123173768001 ) ) ;
#6009 = AXIS2_PLACEMENT_3D ( 'NONE', #19226, #5955, #13957 ) ;
#6010 = AXIS2_PLACEMENT_3D ( 'NONE', #3077, #322, #15021 ) ;
#6011 = CARTESIAN_POINT ( 'NONE',  ( 44.03140696652193498, 63.19948385550240744, -4.306917132069424170 ) ) ;
#6012 = AXIS2_PLACEMENT_3D ( 'NONE', #7430, #5765, #17737 ) ;
#6013 = FACE_OUTER_BOUND ( 'NONE', #15349, .T. ) ;
#6014 = CARTESIAN_POINT ( 'NONE',  ( -20.63749999999999929, 0.000000000000000000, -4.000000000000000000 ) ) ;
#6015 = CARTESIAN_POINT ( 'NONE',  ( 43.34962307344081012, 58.89948385550241028, 2.184720259617164650 ) ) ;
#6016 = CARTESIAN_POINT ( 'NONE',  ( 4.000000000000000888, 1.539600717838996990, -3.300726591567079815 ) ) ;
#6017 = CARTESIAN_POINT ( 'NONE',  ( 42.38452918213188525, 51.09948385550240602, -2.450534656007040013 ) ) ;
#6018 = DIRECTION ( 'NONE',  ( 0.000000000000000000, 0.000000000000000000, -1.000000000000000000 ) ) ;
#6019 = CARTESIAN_POINT ( 'NONE',  ( 49.97728705011495265, 55.50051614449766646, 7.000000000000000888 ) ) ;
#6020 = CARTESIAN_POINT ( 'NONE',  ( -31.74999999999995737, 4.286263797015736595E-16, -3.500000000000000000 ) ) ;
#6021 = ORIENTED_EDGE ( 'NONE', *, *, #6410, .T. ) ;
#6022 = TOROIDAL_SURFACE ( 'NONE', #6945, 5.899999999999999467, 0.1000000000000010186 ) ;
#6023 = ORIENTED_EDGE ( 'NONE', *, *, #18102, .F. ) ;
#6024 = DIRECTION ( 'NONE',  ( 0.000000000000000000, 0.000000000000000000, 1.000000000000000000 ) ) ;
#6025 = ORIENTED_EDGE ( 'NONE', *, *, #18647, .F. ) ;
#6026 = CARTESIAN_POINT ( 'NONE',  ( 2.449293598294706513E-15, -20.00000000000000000, 15.00000000000000355 ) ) ;
#6027 = EDGE_CURVE ( 'NONE', #3032, #3339, #5022, .T. ) ;
#6028 = ORIENTED_EDGE ( 'NONE', *, *, #12926, .F. ) ;
#6029 = CARTESIAN_POINT ( 'NONE',  ( -72.99999999999997158, -3.000000000000000000, 6.000000000000005329 ) ) ;
#6030 = ORIENTED_EDGE ( 'NONE', *, *, #7489, .F. ) ;
#6031 = DIRECTION ( 'NONE',  ( 1.387778780781445676E-16, -1.000000000000000000, 0.000000000000000000 ) ) ;
#6032 = PLANE ( 'NONE',  #16102 ) ;
#6033 = CARTESIAN_POINT ( 'NONE',  ( 56.30877334542961421, 59.99948385550241170, -0.02388180880520959434 ) ) ;
#6034 = FACE_OUTER_BOUND ( 'NONE', #9664, .T. ) ;
#6035 = CARTESIAN_POINT ( 'NONE',  ( -4.799999999999999822, 5.878304635907294211E-16, -1.000000000000000000 ) ) ;
#6036 = CARTESIAN_POINT ( 'NONE',  ( 52.62207051974829852, 50.60051614449765367, -7.992620115222797139 ) ) ;
#6037 = CARTESIAN_POINT ( 'NONE',  ( 55.11794222512599362, 58.80051614449766362, -3.688883143319583446 ) ) ;
#6038 = PLANE ( 'NONE',  #1919 ) ;
#6039 = DIRECTION ( 'NONE',  ( 1.000000000000000000, 0.000000000000000000, 0.000000000000000000 ) ) ;
#6040 = EDGE_LOOP ( 'NONE', ( #5360, #15655 ) ) ;
#6041 = EDGE_CURVE ( 'NONE', #4513, #2192, #2548, .T. ) ;
#6042 = ORIENTED_EDGE ( 'NONE', *, *, #6433, .F. ) ;
#6043 = CARTESIAN_POINT ( 'NONE',  ( 1.925929944387235853E-31, 15.00000000000001599, 9.999999999999998224 ) ) ;
#6044 = EDGE_LOOP ( 'NONE', ( #13587, #245, #1737, #252 ) ) ;
#6045 = CARTESIAN_POINT ( 'NONE',  ( 47.70284917648453415, 65.39948385550239607, -6.992620115222774047 ) ) ;
#6046 = DIRECTION ( 'NONE',  ( 0.04542589977017006536, -0.9989677110047503472, 0.000000000000000000 ) ) ;
#6047 =( GEOMETRIC_REPRESENTATION_CONTEXT ( 3 ) GLOBAL_UNCERTAINTY_ASSIGNED_CONTEXT ( ( #12242 ) ) GLOBAL_UNIT_ASSIGNED_CONTEXT ( ( #11671, #10191, #4326 ) ) REPRESENTATION_CONTEXT ( 'NONE', 'WORKASPACE' ) );
#6048 = ORIENTED_EDGE ( 'NONE', *, *, #6384, .F. ) ;
#6049 = FACE_OUTER_BOUND ( 'NONE', #17142, .T. ) ;
#6050 = EDGE_CURVE ( 'NONE', #9833, #18783, #13169, .T. ) ;
#6051 = EDGE_CURVE ( 'NONE', #6699, #5816, #331, .T. ) ;
#6052 = ORIENTED_EDGE ( 'NONE', *, *, #2938, .F. ) ;
#6053 = FACE_OUTER_BOUND ( 'NONE', #10844, .T. ) ;
#6054 = VERTEX_POINT ( 'NONE', #18253 ) ;
#6055 = CARTESIAN_POINT ( 'NONE',  ( 43.20883090819745576, 46.79948385550240886, 4.963592699179006473 ) ) ;
#6056 = CARTESIAN_POINT ( 'NONE',  ( 51.88965917396063077, 45.00000000000000711, -6.239765512074564313 ) ) ;
#6057 = CARTESIAN_POINT ( 'NONE',  ( 54.13287192849676188, 58.29948385550240175, 5.649768623646098220 ) ) ;
#6058 = PLANE ( 'NONE',  #19287 ) ;
#6059 = PRESENTATION_STYLE_ASSIGNMENT (( #1654 ) ) ;
#6060 = CARTESIAN_POINT ( 'NONE',  ( 44.03140696652198471, 55.80051614449766362, 4.306917132069485454 ) ) ;
#6061 = CARTESIAN_POINT ( 'NONE',  ( 2.321707774797442170, -4.824281976789052351, -0.8000000000000000444 ) ) ;
#6062 = EDGE_CURVE ( 'NONE', #7928, #10265, #12537, .T. ) ;
#6063 = DIRECTION ( 'NONE',  ( -0.000000000000000000, -0.000000000000000000, 1.000000000000000000 ) ) ;
#6064 = EDGE_CURVE ( 'NONE', #14568, #11186, #10962, .T. ) ;
#6065 = DIRECTION ( 'NONE',  ( 1.000000000000000000, 0.000000000000000000, 0.000000000000000000 ) ) ;
#6066 = VERTEX_POINT ( 'NONE', #1963 ) ;
#6067 = ADVANCED_FACE ( 'NONE', ( #13812 ), #18349, .T. ) ;
#6068 = EDGE_LOOP ( 'NONE', ( #4305, #15464, #9179, #15341, #14394, #9518, #1436 ) ) ;
#6069 = VERTEX_POINT ( 'NONE', #12534 ) ;
#6070 = DIRECTION ( 'NONE',  ( 0.000000000000000000, 0.000000000000000000, -1.000000000000000000 ) ) ;
#6071 = FILL_AREA_STYLE ('',( #6156 ) ) ;
#6072 = CARTESIAN_POINT ( 'NONE',  ( 45.90387839640214196, 46.69948385550240744, 5.676469297603166098 ) ) ;
#6073 = LINE ( 'NONE', #12041, #15299 ) ;
#6074 = ORIENTED_EDGE ( 'NONE', *, *, #7614, .T. ) ;
#6075 = FACE_OUTER_BOUND ( 'NONE', #8734, .T. ) ;
#6076 = ORIENTED_EDGE ( 'NONE', *, *, #116, .F. ) ;
#6077 = CARTESIAN_POINT ( 'NONE',  ( 43.34962307344078880, 62.10051614449766078, -2.184720259617096705 ) ) ;
#6078 = ORIENTED_EDGE ( 'NONE', *, *, #18085, .F. ) ;
#6079 = CARTESIAN_POINT ( 'NONE',  ( -32.00000000000000000, -3.000000000000000000, -5.999999999999998224 ) ) ;
#6080 = DIRECTION ( 'NONE',  ( -0.9914448613738102711, -0.1305261922200524338, 0.000000000000000000 ) ) ;
#6081 = CARTESIAN_POINT ( 'NONE',  ( 48.07319477248762496, 54.40051614449765793, -6.007379884777208190 ) ) ;
#6082 = FACE_OUTER_BOUND ( 'NONE', #17872, .T. ) ;
#6083 = VECTOR ( 'NONE', #12695, 1000.000000000000000 ) ;
#6084 = CARTESIAN_POINT ( 'NONE',  ( 51.97223112728254790, 58.39948385550241028, 5.992620115222778487 ) ) ;
#6085 = CARTESIAN_POINT ( 'NONE',  ( -17.85000000000000142, -19.99999999999999289, -20.00000000000000000 ) ) ;
#6086 = AXIS2_PLACEMENT_3D ( 'NONE', #8352, #10203, #17687 ) ;
#6087 = CARTESIAN_POINT ( 'NONE',  ( 42.39856655714564226, 52.10051614449766788, -2.493737253992044156 ) ) ;
#6088 = CARTESIAN_POINT ( 'NONE',  ( 6.367873360227559232, -5.773502691896263528, 0.000000000000000000 ) ) ;
#6089 = CARTESIAN_POINT ( 'NONE',  ( 4.030867648405251025, 2.329326259789668452, -2.965488570640744115 ) ) ;
#6090 = VERTEX_POINT ( 'NONE', #15473 ) ;
#6091 = DIRECTION ( 'NONE',  ( 1.000000000000000000, 0.000000000000000000, 0.000000000000000000 ) ) ;
#6092 = EDGE_CURVE ( 'NONE', #3574, #11553, #2848, .T. ) ;
#6093 = APPLICATION_PROTOCOL_DEFINITION ( 'draft international standard', 'automotive_design', 1998, #8877 ) ;
#6094 = EDGE_LOOP ( 'NONE', ( #2266, #6456, #1154, #1279 ) ) ;
#6095 = CARTESIAN_POINT ( 'NONE',  ( 6.897297840755645792E-16, -2.686816014504582739, -2.346298152288354366 ) ) ;
#6096 = EDGE_CURVE ( 'NONE', #16847, #2940, #18546, .T. ) ;
#6097 = CARTESIAN_POINT ( 'NONE',  ( 0.000000000000000000, 0.000000000000000000, 0.000000000000000000 ) ) ;
#6098 = VECTOR ( 'NONE', #7276, 1000.000000000000000 ) ;
#6099 = CARTESIAN_POINT ( 'NONE',  ( 44.05948171654949874, 64.79948385550240175, 4.345558710429104465 ) ) ;
#6100 = CARTESIAN_POINT ( 'NONE',  ( 4.747884751462026820, -5.143694235355983579, 0.000000000000000000 ) ) ;
#6101 = DIRECTION ( 'NONE',  ( 0.000000000000000000, -0.000000000000000000, 1.000000000000000000 ) ) ;
#6102 = DIRECTION ( 'NONE',  ( 1.000000000000000000, 0.000000000000000000, 0.000000000000000000 ) ) ;
#6103 = CARTESIAN_POINT ( 'NONE',  ( 49.97728705011488159, 59.49948385550240459, -7.000000000000000888 ) ) ;
#6104 = CARTESIAN_POINT ( 'NONE',  ( -10.75570504584948139, -3.819660112501066518, -9.000000000000000000 ) ) ;
#6105 = CARTESIAN_POINT ( 'NONE',  ( 42.38452918213188525, 55.09948385550241312, -2.450534656007040013 ) ) ;
#6106 = CARTESIAN_POINT ( 'NONE',  ( 3.950241966888156320, -2.668221755853644073, -2.378504353000863158 ) ) ;
#6107 = CARTESIAN_POINT ( 'NONE',  ( 54.09612160359792199, 55.30051614449765651, 5.676469297603124353 ) ) ;
#6108 = FACE_OUTER_BOUND ( 'NONE', #13171, .T. ) ;
#6109 = CIRCLE ( 'NONE', #14233, 8.099999999999999645 ) ;
#6110 = VERTEX_POINT ( 'NONE', #1769 ) ;
#6111 = ADVANCED_FACE ( 'NONE', ( #16869 ), #6452, .T. ) ;
#6112 = VERTEX_POINT ( 'NONE', #7834 ) ;
#6113 = CIRCLE ( 'NONE', #11103, 10.00000000000000888 ) ;
#6114 = CARTESIAN_POINT ( 'NONE',  ( -3.974344831685191280E-13, 4.796734841935104576, -3.721909803043223608 ) ) ;
#6115 = ORIENTED_EDGE ( 'NONE', *, *, #5327, .T. ) ;
#6116 = DIRECTION ( 'NONE',  ( 1.000000000000000000, 0.000000000000000000, 0.000000000000000000 ) ) ;
#6117 = CARTESIAN_POINT ( 'NONE',  ( 54.13287192849676188, 62.29948385550240886, 5.649768623646098220 ) ) ;
#6118 = DIRECTION ( 'NONE',  ( 0.000000000000000000, 8.673617379884036458E-16, 1.000000000000000000 ) ) ;
#6119 = ORIENTED_EDGE ( 'NONE', *, *, #14107, .T. ) ;
#6120 = CARTESIAN_POINT ( 'NONE',  ( 62.49999999999998579, 5.000000000000018652, -5.000000000000000000 ) ) ;
#6121 = CARTESIAN_POINT ( 'NONE',  ( -144.9999999999999716, -14.99999999999999467, -4.000000000000000000 ) ) ;
#6122 = CARTESIAN_POINT ( 'NONE',  ( 51.97223112728254790, 54.39948385550241028, 5.992620115222778487 ) ) ;
#6123 = CARTESIAN_POINT ( 'NONE',  ( -54.99999999999996447, -22.99999999999998579, -10.00000000000000000 ) ) ;
#6124 = LINE ( 'NONE', #14943, #3380 ) ;
#6125 = CARTESIAN_POINT ( 'NONE',  ( 43.18075615816994173, 51.80051614449766362, 4.924951120819380357 ) ) ;
#6126 = AXIS2_PLACEMENT_3D ( 'NONE', #3723, #14300, #4907 ) ;
#6127 = CARTESIAN_POINT ( 'NONE',  ( 44.28664221472221385, 53.90051614449765793, 1.832500667257213722 ) ) ;
#6128 = CARTESIAN_POINT ( 'NONE',  ( -54.99999999999996447, -6.999999999999985789, 10.00000000000000000 ) ) ;
#6129 = CARTESIAN_POINT ( 'NONE',  ( 19.97007065299863271, -21.09374499507102740, 9.000000000000000000 ) ) ;
#6130 = EDGE_LOOP ( 'NONE', ( #5498, #11202 ) ) ;
#6131 = ORIENTED_EDGE ( 'NONE', *, *, #17858, .F. ) ;
#6132 = ORIENTED_EDGE ( 'NONE', *, *, #17016, .F. ) ;
#6133 = CARTESIAN_POINT ( 'NONE',  ( 45.86712807150323812, 65.29948385550241596, -5.649768623646098220 ) ) ;
#6134 = CARTESIAN_POINT ( 'NONE',  ( -0.1713913650100259145, 0.000000000000000000, 5.575000000000000178 ) ) ;
#6135 = VERTEX_POINT ( 'NONE', #13718 ) ;
#6136 = CARTESIAN_POINT ( 'NONE',  ( 0.000000000000000000, 0.000000000000000000, 0.000000000000000000 ) ) ;
#6137 = AXIS2_PLACEMENT_3D ( 'NONE', #11742, #8416, #5388 ) ;
#6138 = CARTESIAN_POINT ( 'NONE',  ( 2.449293598294706513E-15, -20.00000000000000000, 9.000000000000000000 ) ) ;
#6139 = ORIENTED_EDGE ( 'NONE', *, *, #3057, .T. ) ;
#6140 = DIRECTION ( 'NONE',  ( -1.000000000000000000, -0.000000000000000000, -0.000000000000000000 ) ) ;
#6141 = VERTEX_POINT ( 'NONE', #3434 ) ;
#6142 = CARTESIAN_POINT ( 'NONE',  ( 47.42335538002188144, 48.59948385550239891, 8.007379884777233059 ) ) ;
#6143 = CARTESIAN_POINT ( 'NONE',  ( -1.149999999999998135, 4.898587196589412829E-16, 4.000000000000000000 ) ) ;
#6144 = CARTESIAN_POINT ( 'NONE',  ( 42.63976443033212860, 56.99948385550241170, 0.02388180880522514787 ) ) ;
#6145 = DIRECTION ( 'NONE',  ( -0.000000000000000000, -0.000000000000000000, 1.000000000000000000 ) ) ;
#6146 = AXIS2_PLACEMENT_3D ( 'NONE', #8429, #14503, #1087 ) ;
#6147 = CARTESIAN_POINT ( 'NONE',  ( 57.36023556966787851, 57.00051614449766646, 0.02388180880515038476 ) ) ;
#6148 = DIRECTION ( 'NONE',  ( 0.000000000000000000, 0.000000000000000000, 1.000000000000000000 ) ) ;
#6149 = CARTESIAN_POINT ( 'NONE',  ( -158.9999999999999716, -14.99999999999999645, 15.00000000000000000 ) ) ;
#6150 = CARTESIAN_POINT ( 'NONE',  ( -4.211405944401398038, -2.460460786169389902, -3.751298493805494072 ) ) ;
#6151 = ORIENTED_EDGE ( 'NONE', *, *, #9312, .T. ) ;
#6152 = EDGE_CURVE ( 'NONE', #10243, #3495, #679, .T. ) ;
#6153 = ORIENTED_EDGE ( 'NONE', *, *, #1853, .F. ) ;
#6154 = VERTEX_POINT ( 'NONE', #5088 ) ;
#6155 = FACE_OUTER_BOUND ( 'NONE', #7996, .T. ) ;
#6156 = FILL_AREA_STYLE_COLOUR ( '', #18458 ) ;
#6157 = EDGE_CURVE ( 'NONE', #12615, #4769, #2078, .T. ) ;
#6158 = CARTESIAN_POINT ( 'NONE',  ( 52.25172492374522903, 45.59948385550240602, -7.007379884777225953 ) ) ;
#6159 = FACE_OUTER_BOUND ( 'NONE', #17245, .T. ) ;
#6160 = ORIENTED_EDGE ( 'NONE', *, *, #10585, .T. ) ;
#6161 = CARTESIAN_POINT ( 'NONE',  ( 6.506987859255521478, 5.850751062354592413, 1.196609732200561596E-15 ) ) ;
#6162 = EDGE_CURVE ( 'NONE', #3362, #9866, #6363, .T. ) ;
#6163 = EDGE_CURVE ( 'NONE', #5141, #2940, #2232, .T. ) ;
#6164 = ORIENTED_EDGE ( 'NONE', *, *, #17255, .T. ) ;
#6165 = ADVANCED_BREP_SHAPE_REPRESENTATION ( '', ( #8395, #10359 ), #10908 ) ;
#6166 = CARTESIAN_POINT ( 'NONE',  ( 44.05948171654945611, 60.20051614449765509, -4.345558710429044069 ) ) ;
#6167 = ORIENTED_EDGE ( 'NONE', *, *, #13705, .T. ) ;
#6168 = CIRCLE ( 'NONE', #13047, 0.9999999999999993339 ) ;
#6169 = ADVANCED_FACE ( 'NONE', ( #12830, #15971 ), #5377, .F. ) ;
#6170 = CARTESIAN_POINT ( 'NONE',  ( 6.270568613849412998, -3.932080789230354867, 3.401571648088637101 ) ) ;
#6171 = UNCERTAINTY_MEASURE_WITH_UNIT (LENGTH_MEASURE( 1.000000000000000082E-05 ), #10942, 'distance_accuracy_value', 'NONE');
#6172 = DIRECTION ( 'NONE',  ( -0.000000000000000000, -0.000000000000000000, 1.000000000000000000 ) ) ;
#6173 = CARTESIAN_POINT ( 'NONE',  ( 56.30877334542961421, 57.00051614449766646, 0.02388180880515774693 ) ) ;
#6174 = CARTESIAN_POINT ( 'NONE',  ( 0.1983443223721567394, 3.359771601077105707, -4.180704885107416224 ) ) ;
#6175 = AXIS2_PLACEMENT_3D ( 'NONE', #6100, #1691, #10403 ) ;
#6176 = FILL_AREA_STYLE ('',( #8916 ) ) ;
#6177 = CARTESIAN_POINT ( 'NONE',  ( 48.02776887271745210, 57.39948385550241028, -5.992620115222778487 ) ) ;
#6178 = CARTESIAN_POINT ( 'NONE',  ( 0.000000000000000000, 20.00000000000001421, -9.999999999999998224 ) ) ;
#6179 = EDGE_CURVE ( 'NONE', #13491, #17135, #12376, .T. ) ;
#6180 = CARTESIAN_POINT ( 'NONE',  ( 57.61547081786810764, 50.90051614449765793, -2.450534656007114176 ) ) ;
#6181 = CARTESIAN_POINT ( 'NONE',  ( -4.000000000000000000, -0.7890432684750890990, -0.04868663549882315533 ) ) ;
#6182 = VECTOR ( 'NONE', #16036, 1000.000000000000000 ) ;
#6183 = CYLINDRICAL_SURFACE ( 'NONE', #5204, 20.00000000000000000 ) ;
#6184 = ADVANCED_FACE ( 'NONE', ( #7140 ), #15777, .F. ) ;
#6185 = VERTEX_POINT ( 'NONE', #5277 ) ;
#6186 = DIRECTION ( 'NONE',  ( -1.000000000000000000, 0.000000000000000000, 0.000000000000000000 ) ) ;
#6187 = CIRCLE ( 'NONE', #9599, 14.00000000000000000 ) ;
#6188 = ORIENTED_EDGE ( 'NONE', *, *, #17675, .T. ) ;
#6189 = LINE ( 'NONE', #12064, #7988 ) ;
#6190 = CARTESIAN_POINT ( 'NONE',  ( 0.000000000000000000, 0.000000000000000000, 0.000000000000000000 ) ) ;
#6191 = VECTOR ( 'NONE', #326, 1000.000000000000000 ) ;
#6192 = CARTESIAN_POINT ( 'NONE',  ( 43.33558569842703179, 63.09948385550240602, -2.141517661632099223 ) ) ;
#6193 = DIRECTION ( 'NONE',  ( -2.191393683118470056E-17, -7.538405132783724027E-17, -1.000000000000000000 ) ) ;
#6194 = CIRCLE ( 'NONE', #9303, 2.149999999999999023 ) ;
#6195 = CARTESIAN_POINT ( 'NONE',  ( -19.02113032590304442, -26.18033988749903074, -9.000000000000000000 ) ) ;
#6196 = DIRECTION ( 'NONE',  ( 1.000000000000000000, 0.000000000000000000, 0.000000000000000000 ) ) ;
#6197 = CARTESIAN_POINT ( 'NONE',  ( 45.90387839640214196, 56.69948385550240744, 5.676469297603166098 ) ) ;
#6198 = DIRECTION ( 'NONE',  ( 0.000000000000000000, 0.000000000000000000, 1.000000000000000000 ) ) ;
#6199 = CARTESIAN_POINT ( 'NONE',  ( 56.79116909180255135, 55.79948385550239465, -4.963592699179005585 ) ) ;
#6200 = CARTESIAN_POINT ( 'NONE',  ( -19.97007065299861850, -18.90625500492883759, 9.000000000000000000 ) ) ;
#6201 = CARTESIAN_POINT ( 'NONE',  ( 52.29715082351538769, 54.60051614449766788, -6.992620115222796251 ) ) ;
#6202 = CIRCLE ( 'NONE', #5255, 4.000000000000021316 ) ;
#6203 = CARTESIAN_POINT ( 'NONE',  ( -54.99999999999996447, -22.99999999999998579, 15.00000000000000000 ) ) ;
#6204 = CIRCLE ( 'NONE', #16544, 7.900000000000002132 ) ;
#6205 = APPLICATION_PROTOCOL_DEFINITION ( 'draft international standard', 'automotive_design', 1998, #10022 ) ;
#6206 = ORIENTED_EDGE ( 'NONE', *, *, #1633, .T. ) ;
#6207 = CARTESIAN_POINT ( 'NONE',  ( 2.100000000000000089, 0.000000000000000000, -5.000000000000000000 ) ) ;
#6208 = CARTESIAN_POINT ( 'NONE',  ( 56.65037692655921120, 49.10051614449766078, 2.184720259617097593 ) ) ;
#6209 = CARTESIAN_POINT ( 'NONE',  ( 45.90387839640214196, 64.69948385550240744, 5.676469297603166098 ) ) ;
#6210 = DIRECTION ( 'NONE',  ( -9.710251638871371392E-17, -5.969973981896233748E-17, -1.000000000000000000 ) ) ;
#6211 = ORIENTED_EDGE ( 'NONE', *, *, #19024, .F. ) ;
#6212 = LINE ( 'NONE', #1517, #7714 ) ;
#6213 = AXIS2_PLACEMENT_3D ( 'NONE', #18139, #8710, #4304 ) ;
#6214 = DIRECTION ( 'NONE',  ( 1.000000000000000000, 0.000000000000000000, 0.000000000000000000 ) ) ;
#6215 = EDGE_CURVE ( 'NONE', #7491, #10940, #11594, .T. ) ;
#6216 = AXIS2_PLACEMENT_3D ( 'NONE', #15292, #1873, #15196 ) ;
#6217 = CARTESIAN_POINT ( 'NONE',  ( 48.02776887271745210, 57.39948385550241028, -5.992620115222778487 ) ) ;
#6218 = CARTESIAN_POINT ( 'NONE',  ( 1.000000000000002442, -20.00000000000000000, 8.999999999999998224 ) ) ;
#6219 = CARTESIAN_POINT ( 'NONE',  ( -0.4472135954999577612, 0.000000000000000000, 0.000000000000000000 ) ) ;
#6220 = CARTESIAN_POINT ( 'NONE',  ( 43.18075615816994173, 55.80051614449766362, 4.924951120819380357 ) ) ;
#6221 = EDGE_CURVE ( 'NONE', #6930, #508, #5331, .T. ) ;
#6222 = CARTESIAN_POINT ( 'NONE',  ( 51.92680522751238925, 55.40051614449767214, 6.007379884777208190 ) ) ;
#6223 = DIRECTION ( 'NONE',  ( 1.000000000000000000, 0.000000000000000000, 0.000000000000000000 ) ) ;
#6224 = CARTESIAN_POINT ( 'NONE',  ( 6.245824673232814206, -3.903127342723638371, -3.450227696316022996 ) ) ;
#6225 = EDGE_LOOP ( 'NONE', ( #491, #5233, #9689, #6313 ) ) ;
#6226 = EDGE_LOOP ( 'NONE', ( #14073, #17585, #6990, #18522 ) ) ;
#6227 = CARTESIAN_POINT ( 'NONE',  ( -19.02113032590308705, -13.81966011250110249, -9.000000000000000000 ) ) ;
#6228 = ORIENTED_EDGE ( 'NONE', *, *, #16237, .T. ) ;
#6229 = AXIS2_PLACEMENT_3D ( 'NONE', #5262, #2542, #8204 ) ;
#6230 = CONICAL_SURFACE ( 'NONE', #286, 3.500000000000000000, 1.047197551196600296 ) ;
#6231 = FACE_OUTER_BOUND ( 'NONE', #2049, .T. ) ;
#6232 = ORIENTED_EDGE ( 'NONE', *, *, #11953, .T. ) ;
#6233 = DIRECTION ( 'NONE',  ( 1.000000000000000000, 0.000000000000000000, 0.000000000000000000 ) ) ;
#6234 = CARTESIAN_POINT ( 'NONE',  ( 56.66441430157296821, 50.09948385550240602, 2.141517661632100111 ) ) ;
#6235 = ORIENTED_EDGE ( 'NONE', *, *, #19014, .T. ) ;
#6236 = AXIS2_PLACEMENT_3D ( 'NONE', #18664, #8241, #15900 ) ;
#6237 = LINE ( 'NONE', #4775, #3494 ) ;
#6238 = ORIENTED_EDGE ( 'NONE', *, *, #17697, .T. ) ;
#6239 = CARTESIAN_POINT ( 'NONE',  ( 45.31609314410967926, 46.69948385550240744, 6.485486291978119766 ) ) ;
#6240 = CARTESIAN_POINT ( 'NONE',  ( -10.75570504584937304, -36.18033988749900942, -9.000000000000000000 ) ) ;
#6241 = CARTESIAN_POINT ( 'NONE',  ( 49.97728705011488159, 59.49948385550240459, -7.000000000000000888 ) ) ;
#6242 = CARTESIAN_POINT ( 'NONE',  ( -19.30627432446643610, -25.22185519795866782, 9.000000000000000000 ) ) ;
#6243 = CARTESIAN_POINT ( 'NONE',  ( 52.25172492374527877, 57.40051614449765083, 7.007379884777203749 ) ) ;
#6244 = VECTOR ( 'NONE', #6704, 1000.000000000000000 ) ;
#6245 = AXIS2_PLACEMENT_3D ( 'NONE', #5647, #4475, #4180 ) ;
#6246 = LINE ( 'NONE', #6342, #13203 ) ;
#6247 = CARTESIAN_POINT ( 'NONE',  ( 6.534533895392296010, -5.902695350657468865, 6.631005141235907328E-15 ) ) ;
#6248 = ORIENTED_EDGE ( 'NONE', *, *, #17454, .T. ) ;
#6249 = ORIENTED_EDGE ( 'NONE', *, *, #5939, .F. ) ;
#6250 = VERTEX_POINT ( 'NONE', #16073 ) ;
#6251 = DIRECTION ( 'NONE',  ( 0.000000000000000000, 0.000000000000000000, 1.000000000000000000 ) ) ;
#6252 = SURFACE_STYLE_FILL_AREA ( #6071 ) ;
#6253 = CARTESIAN_POINT ( 'NONE',  ( 49.97728705011488159, 51.49948385550240459, -7.000000000000000888 ) ) ;
#6254 = DIRECTION ( 'NONE',  ( 0.000000000000000000, -0.000000000000000000, 1.000000000000000000 ) ) ;
#6255 = ORIENTED_EDGE ( 'NONE', *, *, #2996, .T. ) ;
#6256 = CARTESIAN_POINT ( 'NONE',  ( -4.000000000000000000, -2.309401076758512694, -3.433295621305382461 ) ) ;
#6257 = CIRCLE ( 'NONE', #15015, 1.999999999999998224 ) ;
#6258 = ORIENTED_EDGE ( 'NONE', *, *, #10215, .F. ) ;
#6259 = CARTESIAN_POINT ( 'NONE',  ( 57.36023556966787851, 61.00051614449765935, 0.02388180880515038476 ) ) ;
#6260 = ORIENTED_EDGE ( 'NONE', *, *, #6626, .F. ) ;
#6261 = EDGE_CURVE ( 'NONE', #6141, #5579, #3168, .T. ) ;
#6262 = DIRECTION ( 'NONE',  ( -1.000000000000000000, 0.000000000000000000, 0.000000000000000000 ) ) ;
#6263 = CARTESIAN_POINT ( 'NONE',  ( 2.449293598294706513E-15, -20.00000000000000000, -20.00000000000000000 ) ) ;
#6264 = PRODUCT_DEFINITION ( 'UNKNOWN', '', #1038, #9291 ) ;
#6265 = CARTESIAN_POINT ( 'NONE',  ( 51.97223112728249816, 52.60051614449765367, -5.992620115222793586 ) ) ;
#6266 = DIRECTION ( 'NONE',  ( 0.000000000000000000, 0.000000000000000000, 1.000000000000000000 ) ) ;
#6267 = DIRECTION ( 'NONE',  ( -1.000000000000000000, -0.000000000000000000, -0.000000000000000000 ) ) ;
#6268 = CARTESIAN_POINT ( 'NONE',  ( 55.11794222512601493, 64.19948385550240744, 3.688883143319541702 ) ) ;
#6269 = CARTESIAN_POINT ( 'NONE',  ( 6.244889965166093404, 4.918546365148221078, -1.691415889817839302 ) ) ;
#6270 = CONICAL_SURFACE ( 'NONE', #12521, 3.500000000000000000, 1.047197551196600296 ) ;
#6271 = CARTESIAN_POINT ( 'NONE',  ( 45.27934281921082516, 51.70051614449765509, 6.458785618021089192 ) ) ;
#6272 = DIRECTION ( 'NONE',  ( -1.000000000000000000, -4.082155997157843695E-16, 0.000000000000000000 ) ) ;
#6273 = CIRCLE ( 'NONE', #14408, 20.00000000000000000 ) ;
#6274 = ORIENTED_EDGE ( 'NONE', *, *, #8736, .F. ) ;
#6275 = CARTESIAN_POINT ( 'NONE',  ( 22.00000000000000000, -20.00000000000000000, -12.00000000000000000 ) ) ;
#6276 = SHAPE_REPRESENTATION_RELATIONSHIP ( 'NONE' , 'NONE' ,  #659, #8491 ) ;
#6277 = ORIENTED_EDGE ( 'NONE', *, *, #5984, .F. ) ;
#6278 = ADVANCED_FACE ( 'NONE', ( #3716, #971 ), #17354, .F. ) ;
#6279 = CARTESIAN_POINT ( 'NONE',  ( 4.175813232069147674, 2.061359961916367833, 3.570380186727398097 ) ) ;
#6280 = SHAPE_DEFINITION_REPRESENTATION ( #14460, #659 ) ;
#6281 = EDGE_CURVE ( 'NONE', #17942, #15146, #8465, .T. ) ;
#6282 = VECTOR ( 'NONE', #128, 1000.000000000000000 ) ;
#6283 = ORIENTED_EDGE ( 'NONE', *, *, #16061, .F. ) ;
#6284 = CARTESIAN_POINT ( 'NONE',  ( 0.1217565302851044418, -2.351289329882175760, -2.927447417349501535 ) ) ;
#6285 = DIRECTION ( 'NONE',  ( 0.000000000000000000, 0.000000000000000000, 1.000000000000000000 ) ) ;
#6286 = APPLICATION_CONTEXT ( 'automotive_design' ) ;
#6287 = AXIS2_PLACEMENT_3D ( 'NONE', #3833, #2068, #9795 ) ;
#6288 = EDGE_CURVE ( 'NONE', #17511, #2792, #2654, .T. ) ;
#6289 = DIRECTION ( 'NONE',  ( 0.000000000000000000, 0.000000000000000000, -1.000000000000000000 ) ) ;
#6290 = EDGE_CURVE ( 'NONE', #2561, #17889, #3465, .T. ) ;
#6291 = AXIS2_PLACEMENT_3D ( 'NONE', #13878, #3315, #9272 ) ;
#6292 = LINE ( 'NONE', #1884, #14609 ) ;
#6293 = VECTOR ( 'NONE', #5427, 1000.000000000000000 ) ;
#6294 = DIRECTION ( 'NONE',  ( 0.000000000000000000, 0.000000000000000000, -1.000000000000000000 ) ) ;
#6295 = CARTESIAN_POINT ( 'NONE',  ( 0.000000000000000000, 0.000000000000000000, -1.000000000000000000 ) ) ;
#6296 = CARTESIAN_POINT ( 'NONE',  ( 43.33558569842703179, 57.09948385550240602, -2.141517661632099223 ) ) ;
#6297 =( GEOMETRIC_REPRESENTATION_CONTEXT ( 3 ) GLOBAL_UNCERTAINTY_ASSIGNED_CONTEXT ( ( #3426 ) ) GLOBAL_UNIT_ASSIGNED_CONTEXT ( ( #5894, #19054, #8731 ) ) REPRESENTATION_CONTEXT ( 'NONE', 'WORKASPACE' ) );
#6298 = DIRECTION ( 'NONE',  ( -0.000000000000000000, -0.000000000000000000, -1.000000000000000000 ) ) ;
#6299 = CARTESIAN_POINT ( 'NONE',  ( 56.79116909180255135, 59.79948385550240175, -4.963592699179005585 ) ) ;
#6300 = CARTESIAN_POINT ( 'NONE',  ( 56.65037692655921120, 53.10051614449766078, 2.184720259617097593 ) ) ;
#6301 = EDGE_CURVE ( 'NONE', #9525, #12297, #14387, .T. ) ;
#6302 = EDGE_CURVE ( 'NONE', #671, #9948, #3914, .T. ) ;
#6303 = PLANE ( 'NONE',  #9311 ) ;
#6304 = LINE ( 'NONE', #10606, #15687 ) ;
#6305 = EDGE_CURVE ( 'NONE', #2946, #4089, #18512, .T. ) ;
#6306 = CIRCLE ( 'NONE', #18547, 20.00000000000000000 ) ;
#6307 = ORIENTED_EDGE ( 'NONE', *, *, #7307, .T. ) ;
#6308 = TOROIDAL_SURFACE ( 'NONE', #7244, 2.200000000000001066, 0.2000000000000000111 ) ;
#6309 = CARTESIAN_POINT ( 'NONE',  ( -9.037824375505568497, -2.158539001597504559, -9.000000000000000000 ) ) ;
#6310 = CARTESIAN_POINT ( 'NONE',  ( 49.97728705011495265, 45.50051614449765935, 7.000000000000000888 ) ) ;
#6311 = CARTESIAN_POINT ( 'NONE',  ( 52.29715082351547295, 64.39948385550239607, 6.992620115222774047 ) ) ;
#6312 = CARTESIAN_POINT ( 'NONE',  ( 20.00000000000000000, -14.99999999999999289, -23.00000000000000000 ) ) ;
#6313 = ORIENTED_EDGE ( 'NONE', *, *, #14182, .T. ) ;
#6314 = DIRECTION ( 'NONE',  ( -0.000000000000000000, -0.000000000000000000, 1.000000000000000000 ) ) ;
#6315 = DIRECTION ( 'NONE',  ( 1.000000000000000000, 0.000000000000000000, 0.000000000000000000 ) ) ;
#6316 = CARTESIAN_POINT ( 'NONE',  ( 55.69932041026405045, 45.10051614449766788, 1.875703265242156359 ) ) ;
#6317 = CARTESIAN_POINT ( 'NONE',  ( 4.000000000000003553, -2.309401076758513138, -3.504271511726786859 ) ) ;
#6318 = PLANE ( 'NONE',  #12056 ) ;
#6319 = VECTOR ( 'NONE', #5294, 1000.000000000000000 ) ;
#6320 = CARTESIAN_POINT ( 'NONE',  ( 54.72065718078918906, 58.70051614449765509, -6.458785618021089192 ) ) ;
#6321 = CARTESIAN_POINT ( 'NONE',  ( 49.97728705011494554, 55.50051614449766646, 6.000000000000000888 ) ) ;
#6322 = AXIS2_PLACEMENT_3D ( 'NONE', #16657, #15359, #13689 ) ;
#6323 = PLANE ( 'NONE',  #8810 ) ;
#6324 = DIRECTION ( 'NONE',  ( 0.000000000000000000, 0.000000000000000000, 1.000000000000000000 ) ) ;
#6325 = ORIENTED_EDGE ( 'NONE', *, *, #195, .F. ) ;
#6326 = ORIENTED_EDGE ( 'NONE', *, *, #14802, .F. ) ;
#6327 = CARTESIAN_POINT ( 'NONE',  ( 6.390821132688881967, 3.013780087859769363, -5.000000000000000000 ) ) ;
#6328 = VERTEX_POINT ( 'NONE', #4107 ) ;
#6329 = EDGE_CURVE ( 'NONE', #660, #17716, #11443, .T. ) ;
#6330 = ORIENTED_EDGE ( 'NONE', *, *, #16111, .T. ) ;
#6331 = DIRECTION ( 'NONE',  ( -1.000000000000000000, 0.000000000000000000, 0.000000000000000000 ) ) ;
#6332 = EDGE_CURVE ( 'NONE', #10940, #8510, #4096, .T. ) ;
#6333 = CARTESIAN_POINT ( 'NONE',  ( 47.70284917648453415, 51.39948385550240317, -6.992620115222774047 ) ) ;
#6334 = ORIENTED_EDGE ( 'NONE', *, *, #11774, .T. ) ;
#6335 = DIRECTION ( 'NONE',  ( -0.000000000000000000, 1.000000000000000000, -0.000000000000000000 ) ) ;
#6336 = VERTEX_POINT ( 'NONE', #17449 ) ;
#6337 = CARTESIAN_POINT ( 'NONE',  ( 42.39856655714566358, 46.89948385550240317, 2.493737253992119207 ) ) ;
#6338 = CARTESIAN_POINT ( 'NONE',  ( -12.54977455159113475, -35.57251292194792569, -9.000000000000000000 ) ) ;
#6339 = CARTESIAN_POINT ( 'NONE',  ( 51.92680522751233951, 45.59948385550240602, -6.007379884777223289 ) ) ;
#6340 = DIRECTION ( 'NONE',  ( -0.000000000000000000, -0.000000000000000000, 1.000000000000000000 ) ) ;
#6341 = CARTESIAN_POINT ( 'NONE',  ( 45.86712807150329496, 53.70051614449766220, 5.649768623646139964 ) ) ;
#6342 = CARTESIAN_POINT ( 'NONE',  ( 15.51323935927256237, -7.377028694403341191, 0.000000000000000000 ) ) ;
#6343 = CIRCLE ( 'NONE', #12284, 5.000000000000007994 ) ;
#6344 = CARTESIAN_POINT ( 'NONE',  ( 55.94051828345050836, 53.79948385550238754, -4.345558710429104465 ) ) ;
#6345 = CARTESIAN_POINT ( 'NONE',  ( 6.506987859255521478, -5.850751062354593302, 2.176274696337492837E-17 ) ) ;
#6346 = ORIENTED_EDGE ( 'NONE', *, *, #7937, .T. ) ;
#6347 = VERTEX_POINT ( 'NONE', #4006 ) ;
#6348 = DIRECTION ( 'NONE',  ( -0.000000000000000000, -0.000000000000000000, 1.000000000000000000 ) ) ;
#6349 = CARTESIAN_POINT ( 'NONE',  ( 54.09612160359786515, 49.69948385550240744, -5.676469297603166098 ) ) ;
#6350 = LINE ( 'NONE', #9567, #5597 ) ;
#6351 = ORIENTED_EDGE ( 'NONE', *, *, #5063, .T. ) ;
#6352 = DIRECTION ( 'NONE',  ( 1.000000000000000000, 0.000000000000000000, 0.000000000000000000 ) ) ;
#6353 = VERTEX_POINT ( 'NONE', #9968 ) ;
#6354 = CARTESIAN_POINT ( 'NONE',  ( 43.34962307344078880, 60.10051614449766078, -2.184720259617096705 ) ) ;
#6355 = EDGE_LOOP ( 'NONE', ( #1115, #564, #14181, #14168 ) ) ;
#6356 = DIRECTION ( 'NONE',  ( -0.000000000000000000, -0.000000000000000000, -1.000000000000000000 ) ) ;
#6357 = UNCERTAINTY_MEASURE_WITH_UNIT (LENGTH_MEASURE( 1.000000000000000082E-05 ), #5384, 'distance_accuracy_value', 'NONE');
#6358 = DIRECTION ( 'NONE',  ( 0.000000000000000000, 0.000000000000000000, 1.000000000000000000 ) ) ;
#6359 = CARTESIAN_POINT ( 'NONE',  ( 44.88205777487401349, 55.80051614449766362, 3.688883143319584779 ) ) ;
#6360 = CARTESIAN_POINT ( 'NONE',  ( 0.9999999999999997780, -6.008326913195983998, -0.8000000000000000444 ) ) ;
#6361 = LINE ( 'NONE', #18152, #13014 ) ;
#6362 = CARTESIAN_POINT ( 'NONE',  ( 49.97728705011494554, 45.50051614449766646, 6.000000000000000888 ) ) ;
#6363 = LINE ( 'NONE', #13990, #14093 ) ;
#6364 = CARTESIAN_POINT ( 'NONE',  ( 57.60143344285435774, 59.10051614449766078, 2.493737253992045044 ) ) ;
#6365 = ORIENTED_EDGE ( 'NONE', *, *, #1262, .T. ) ;
#6366 = CARTESIAN_POINT ( 'NONE',  ( 0.4465819873851989974, -2.886751345948120218, 4.999999999999999112 ) ) ;
#6367 = ORIENTED_EDGE ( 'NONE', *, *, #3057, .F. ) ;
#6368 = ORIENTED_EDGE ( 'NONE', *, *, #11953, .F. ) ;
#6369 = DIRECTION ( 'NONE',  ( -0.000000000000000000, -0.000000000000000000, 1.000000000000000000 ) ) ;
#6370 = LINE ( 'NONE', #4533, #14080 ) ;
#6371 = AXIS2_PLACEMENT_3D ( 'NONE', #16039, #13083, #1329 ) ;
#6372 = CARTESIAN_POINT ( 'NONE',  ( 55.96859303347805081, 64.19948385550239323, 4.306917132069425058 ) ) ;
#6373 = DIRECTION ( 'NONE',  ( 0.000000000000000000, 0.000000000000000000, 1.000000000000000000 ) ) ;
#6374 = AXIS2_PLACEMENT_3D ( 'NONE', #2605, #5414, #3955 ) ;
#6375 = DIRECTION ( 'NONE',  ( -1.000000000000000000, 0.000000000000000000, 0.000000000000000000 ) ) ;
#6376 = CARTESIAN_POINT ( 'NONE',  ( -32.00000000000000000, -3.000000000000000000, 6.000000000000003553 ) ) ;
#6377 = CARTESIAN_POINT ( 'NONE',  ( 57.36023556966787851, 63.99948385550241881, -0.02388180880522424582 ) ) ;
#6378 = EDGE_CURVE ( 'NONE', #5816, #16278, #8518, .T. ) ;
#6379 = CARTESIAN_POINT ( 'NONE',  ( 0.000000000000000000, 0.5192545390863916310, 0.000000000000000000 ) ) ;
#6380 = CARTESIAN_POINT ( 'NONE',  ( 52.62207051974839089, 62.39948385550240317, 7.992620115222770494 ) ) ;
#6381 = CARTESIAN_POINT ( 'NONE',  ( 50.02271294988505446, 62.50051614449766646, -7.000000000000000888 ) ) ;
#6382 = DIRECTION ( 'NONE',  ( -0.9768494444668812671, -0.2139279384389642935, 0.000000000000000000 ) ) ;
#6383 = DIRECTION ( 'NONE',  ( 1.000000000000000000, 0.000000000000000000, 0.000000000000000000 ) ) ;
#6384 = EDGE_CURVE ( 'NONE', #9638, #1806, #10167, .T. ) ;
#6385 = AXIS2_PLACEMENT_3D ( 'NONE', #7076, #19068, #812 ) ;
#6386 = EDGE_CURVE ( 'NONE', #12421, #950, #19150, .T. ) ;
#6387 = ORIENTED_EDGE ( 'NONE', *, *, #5694, .F. ) ;
#6388 = CIRCLE ( 'NONE', #17063, 20.00000000000000000 ) ;
#6389 = EDGE_CURVE ( 'NONE', #15708, #10950, #7208, .T. ) ;
#6390 = DIRECTION ( 'NONE',  ( -0.000000000000000000, -0.000000000000000000, 1.000000000000000000 ) ) ;
#6391 = CARTESIAN_POINT ( 'NONE',  ( 56.66441430157294690, 44.90051614449765793, -2.141517661632166281 ) ) ;
#6392 = ADVANCED_FACE ( 'NONE', ( #18029 ), #13600, .F. ) ;
#6393 = EDGE_CURVE ( 'NONE', #7648, #7897, #4406, .T. ) ;
#6394 = CARTESIAN_POINT ( 'NONE',  ( 43.34962307344081012, 62.89948385550241028, 2.184720259617164650 ) ) ;
#6395 = CARTESIAN_POINT ( 'NONE',  ( 75.00000000000002842, -39.99999999999998579, 10.00000000000000000 ) ) ;
#6396 = VERTEX_POINT ( 'NONE', #16366 ) ;
#6397 = CARTESIAN_POINT ( 'NONE',  ( 62.49999999999998579, 45.00000000000001421, 15.00000000000000000 ) ) ;
#6398 = CARTESIAN_POINT ( 'NONE',  ( 0.000000000000000000, 0.4273491293402468805, -0.8000000000000000444 ) ) ;
#6399 = CARTESIAN_POINT ( 'NONE',  ( 44.88205777487398507, 63.19948385550240744, -3.688883143319540814 ) ) ;
#6400 = CARTESIAN_POINT ( 'NONE',  ( -14.14213562373094746, -25.00000000000000000, -50.00000000000000000 ) ) ;
#6401 = CARTESIAN_POINT ( 'NONE',  ( -3.158233816355195955, -0.4370479853238878887, -9.000000000000000000 ) ) ;
#6402 = CARTESIAN_POINT ( 'NONE',  ( 57.60143344285435774, 57.10051614449766788, 2.493737253992045044 ) ) ;
#6403 = AXIS2_PLACEMENT_3D ( 'NONE', #11658, #11955, #19241 ) ;
#6404 = CARTESIAN_POINT ( 'NONE',  ( 44.28664221472221385, 57.90051614449765793, 1.832500667257213722 ) ) ;
#6405 = CARTESIAN_POINT ( 'NONE',  ( 2.000000000000000000, -0.8865213383406694847, 1.535500000000001419 ) ) ;
#6406 = DIRECTION ( 'NONE',  ( 0.6691306063588571273, 0.7431448254773952433, 0.000000000000000000 ) ) ;
#6407 = VECTOR ( 'NONE', #5305, 1000.000000000000114 ) ;
#6409 = EDGE_LOOP ( 'NONE', ( #7699, #3579 ) ) ;
#6408 = ADVANCED_FACE ( 'NONE', ( #14875 ), #3296, .F. ) ;
#6410 = EDGE_CURVE ( 'NONE', #11107, #15438, #6273, .T. ) ;
#6411 = VERTEX_POINT ( 'NONE', #17738 ) ;
#6412 = CARTESIAN_POINT ( 'NONE',  ( 54.77701766759913227, 44.74161735293615294, -5.000000000000010658 ) ) ;
#6413 = ORIENTED_EDGE ( 'NONE', *, *, #5168, .F. ) ;
#6414 = CARTESIAN_POINT ( 'NONE',  ( 10.00000000000000000, 25.00000000000001776, 15.00000000000000000 ) ) ;
#6415 = CIRCLE ( 'NONE', #5156, 2.149999999999999023 ) ;
#6416 = ORIENTED_EDGE ( 'NONE', *, *, #18999, .T. ) ;
#6417 = DIRECTION ( 'NONE',  ( -0.000000000000000000, -0.000000000000000000, -1.000000000000000000 ) ) ;
#6418 = CARTESIAN_POINT ( 'NONE',  ( 44.03140696652193498, 55.19948385550240744, -4.306917132069424170 ) ) ;
#6419 = B_SPLINE_CURVE_WITH_KNOTS ( 'NONE', 3,
 ( #8550, #18964, #5213, #3851, #8450, #2598 ),
 .UNSPECIFIED., .F., .F.,
 ( 4, 2, 4 ),
 ( 0.0007315534878134838555, 0.001060812114463466869, 0.001390070741113449884 ),
 .UNSPECIFIED. ) ;
#6420 = VERTEX_POINT ( 'NONE', #14680 ) ;
#6421 = DIRECTION ( 'NONE',  ( 0.000000000000000000, 8.673617379884036458E-16, 1.000000000000000000 ) ) ;
#6422 = VERTEX_POINT ( 'NONE', #2932 ) ;
#6423 = CARTESIAN_POINT ( 'NONE',  ( 57.60143344285433642, 55.89948385550241028, -2.493737253992118319 ) ) ;
#6424 = CARTESIAN_POINT ( 'NONE',  ( 4.180345136606690382, -2.085999704580137060, -3.570468642550115312 ) ) ;
#6425 = CIRCLE ( 'NONE', #9244, 2.649999999999985700 ) ;
#6426 = CARTESIAN_POINT ( 'NONE',  ( 42.63976443033212860, 62.99948385550241170, 0.02388180880522514787 ) ) ;
#6427 = CARTESIAN_POINT ( 'NONE',  ( 0.000000000000000000, 0.4273491293402468805, -0.8000000000000000444 ) ) ;
#6428 = DIRECTION ( 'NONE',  ( 1.000000000000000000, 0.000000000000000000, 0.000000000000000000 ) ) ;
#6429 = CARTESIAN_POINT ( 'NONE',  ( 45.90387839640208512, 58.30051614449766362, -5.676469297603124353 ) ) ;
#6430 = FACE_OUTER_BOUND ( 'NONE', #16684, .T. ) ;
#6431 = CARTESIAN_POINT ( 'NONE',  ( 52.29715082351547295, 58.39948385550238896, 6.992620115222774047 ) ) ;
#6432 = CARTESIAN_POINT ( 'NONE',  ( 6.481779955677436256, -5.820445026626584806, 1.740800559574606662E-15 ) ) ;
#6433 = EDGE_CURVE ( 'NONE', #6054, #14054, #11266, .T. ) ;
#6434 = VERTEX_POINT ( 'NONE', #3028 ) ;
#6435 = CARTESIAN_POINT ( 'NONE',  ( 2.000000000000000000, 0.000000000000000000, 0.000000000000000000 ) ) ;
#6436 = AXIS2_PLACEMENT_3D ( 'NONE', #12043, #7630, #280 ) ;
#6437 = ADVANCED_FACE ( 'NONE', ( #8894 ), #1453, .T. ) ;
#6438 = CARTESIAN_POINT ( 'NONE',  ( 43.34962307344081012, 52.89948385550240317, 2.184720259617164650 ) ) ;
#6439 = SURFACE_STYLE_FILL_AREA ( #1950 ) ;
#6440 = ORIENTED_EDGE ( 'NONE', *, *, #5682, .F. ) ;
#6441 = CARTESIAN_POINT ( 'NONE',  ( 0.1388410611046115850, -3.710337782248037009, -0.5735064479039788665 ) ) ;
#6442 = CIRCLE ( 'NONE', #8947, 0.9999999999999991118 ) ;
#6443 = VERTEX_POINT ( 'NONE', #7235 ) ;
#6444 = CARTESIAN_POINT ( 'NONE',  ( 15.51323935927283237, -32.62297130559633018, -9.000000000000000000 ) ) ;
#6445 = VERTEX_POINT ( 'NONE', #13406 ) ;
#6446 = DIRECTION ( 'NONE',  ( 1.000000000000000000, 0.000000000000000000, 0.000000000000000000 ) ) ;
#6447 = FACE_OUTER_BOUND ( 'NONE', #15532, .T. ) ;
#6448 = CARTESIAN_POINT ( 'NONE',  ( 56.30877334542961421, 63.00051614449766646, 0.02388180880515774693 ) ) ;
#6449 = CARTESIAN_POINT ( 'NONE',  ( -74.99999999999997158, 32.50000000000001421, 9.999999999999998224 ) ) ;
#6450 = EDGE_CURVE ( 'NONE', #14431, #8156, #3789, .T. ) ;
#6451 = CARTESIAN_POINT ( 'NONE',  ( 6.080745460913608902, 0.5192545390863916310, 0.000000000000000000 ) ) ;
#6452 = PLANE ( 'NONE',  #1594 ) ;
#6453 = CARTESIAN_POINT ( 'NONE',  ( 42.39856655714564226, 60.10051614449766788, -2.493737253992044156 ) ) ;
#6454 = ADVANCED_FACE ( 'NONE', ( #5968 ), #10454, .F. ) ;
#6455 = ORIENTED_EDGE ( 'NONE', *, *, #13363, .F. ) ;
#6456 = ORIENTED_EDGE ( 'NONE', *, *, #3903, .T. ) ;
#6457 = FACE_BOUND ( 'NONE', #10508, .T. ) ;
#6458 = ORIENTED_EDGE ( 'NONE', *, *, #404, .F. ) ;
#6459 = DIRECTION ( 'NONE',  ( -0.9135454576425982021, -0.4067366430758060925, 0.000000000000000000 ) ) ;
#6460 = APPLICATION_PROTOCOL_DEFINITION ( 'draft international standard', 'automotive_design', 1998, #14402 ) ;
#6461 = ORIENTED_EDGE ( 'NONE', *, *, #15006, .T. ) ;
#6462 = VECTOR ( 'NONE', #1711, 1000.000000000000000 ) ;
#6463 = CARTESIAN_POINT ( 'NONE',  ( -150.9999999999999432, -14.99999999999999645, 15.79999999999999893 ) ) ;
#6464 = PLANE ( 'NONE',  #17875 ) ;
#6465 = VERTEX_POINT ( 'NONE', #16748 ) ;
#6466 = CARTESIAN_POINT ( 'NONE',  ( -17.32050807568879236, -10.00000000000004263, -9.000000000000000000 ) ) ;
#6467 = DIRECTION ( 'NONE',  ( 0.000000000000000000, 1.224646799147353207E-16, 1.000000000000000000 ) ) ;
#6468 = CARTESIAN_POINT ( 'NONE',  ( -54.99999999999996447, -14.99999999999998579, -10.00000000000000000 ) ) ;
#6469 = B_SPLINE_CURVE_WITH_KNOTS ( 'NONE', 3,
 ( #9576, #2353, #675, #18725 ),
 .UNSPECIFIED., .F., .F.,
 ( 4, 4 ),
 ( 2.380739282169052541E-07, 0.002044882221487534079 ),
 .UNSPECIFIED. ) ;
#6470 = AXIS2_PLACEMENT_3D ( 'NONE', #10421, #6210, #8953 ) ;
#6471 = LINE ( 'NONE', #14010, #8043 ) ;
#6472 = CARTESIAN_POINT ( 'NONE',  ( 50.02271294988512551, 64.49948385550240459, 7.000000000000000888 ) ) ;
#6473 = DIRECTION ( 'NONE',  ( 1.000000000000000000, 0.000000000000000000, 0.000000000000000000 ) ) ;
#6474 = CIRCLE ( 'NONE', #16202, 4.799999999999999822 ) ;
#6475 = CARTESIAN_POINT ( 'NONE',  ( 45.31609314410967926, 60.69948385550240033, 6.485486291978119766 ) ) ;
#6476 = CARTESIAN_POINT ( 'NONE',  ( 42.63976443033212860, 62.00051614449764514, -0.02388180880514948964 ) ) ;
#6477 = FACE_OUTER_BOUND ( 'NONE', #1218, .T. ) ;
#6478 = DIRECTION ( 'NONE',  ( 0.000000000000000000, -0.000000000000000000, 1.000000000000000000 ) ) ;
#6479 = VECTOR ( 'NONE', #912, 1000.000000000000000 ) ;
#6480 = VERTEX_POINT ( 'NONE', #4694 ) ;
#6481 = VECTOR ( 'NONE', #6846, 1000.000000000000000 ) ;
#6482 = CARTESIAN_POINT ( 'NONE',  ( -74.99999999999997158, 20.00000000000001421, 15.00000000000000000 ) ) ;
#6483 = CARTESIAN_POINT ( 'NONE',  ( 57.36023556966787851, 45.00051614449765225, 0.02388180880515038476 ) ) ;
#6484 = DIRECTION ( 'NONE',  ( 0.000000000000000000, 0.000000000000000000, 1.000000000000000000 ) ) ;
#6485 = DIRECTION ( 'NONE',  ( 1.000000000000000000, 0.000000000000000000, 0.000000000000000000 ) ) ;
#6486 = ORIENTED_EDGE ( 'NONE', *, *, #8854, .T. ) ;
#6487 = CYLINDRICAL_SURFACE ( 'NONE', #3346, 5.000000000000000888 ) ;
#6488 = CYLINDRICAL_SURFACE ( 'NONE', #9515, 4.872650870659752442 ) ;
#6489 = EDGE_CURVE ( 'NONE', #16847, #16922, #16953, .T. ) ;
#6490 = CARTESIAN_POINT ( 'NONE',  ( 56.30877334542961421, 61.99948385550241170, -0.02388180880520959434 ) ) ;
#6491 = CARTESIAN_POINT ( 'NONE',  ( 49.99999999999997158, 45.00000000000003553, -7.000000000000000888 ) ) ;
#6492 = CARTESIAN_POINT ( 'NONE',  ( 42.63976443033212860, 46.99948385550240459, 0.02388180880522514787 ) ) ;
#6493 = CARTESIAN_POINT ( 'NONE',  ( -74.99999999999997158, 1.000000000000000000, -5.999999999999998224 ) ) ;
#6494 = CIRCLE ( 'NONE', #14637, 8.000000000000000000 ) ;
#6495 = CARTESIAN_POINT ( 'NONE',  ( 42.39856655714564226, 62.10051614449765367, -2.493737253992044156 ) ) ;
#6496 = CARTESIAN_POINT ( 'NONE',  ( 56.66441430157294690, 44.90051614449765793, -2.141517661632166281 ) ) ;
#6497 = ADVANCED_FACE ( 'NONE', ( #13789 ), #18131, .F. ) ;
#6498 = VECTOR ( 'NONE', #1295, 1000.000000000000000 ) ;
#6499 = CARTESIAN_POINT ( 'NONE',  ( 0.6937372685066666156, -4.453844082567737672, -3.610536846335894445 ) ) ;
#6500 = DIRECTION ( 'NONE',  ( -1.000000000000000000, 0.000000000000000000, 0.000000000000000000 ) ) ;
#6501 = ORIENTED_EDGE ( 'NONE', *, *, #1707, .F. ) ;
#6502 = EDGE_CURVE ( 'NONE', #14591, #4513, #8486, .T. ) ;
#6503 = EDGE_CURVE ( 'NONE', #8420, #17731, #2560, .T. ) ;
#6504 = ORIENTED_EDGE ( 'NONE', *, *, #4133, .F. ) ;
#6505 = CARTESIAN_POINT ( 'NONE',  ( 6.362366615495708366, 2.018765416950190961, -5.108861542006171597 ) ) ;
#6506 = ORIENTED_EDGE ( 'NONE', *, *, #16708, .F. ) ;
#6507 = EDGE_CURVE ( 'NONE', #2689, #17828, #4451, .T. ) ;
#6508 = CARTESIAN_POINT ( 'NONE',  ( -22.00000000000000000, -19.99999999999999289, -20.00000000000000000 ) ) ;
#6509 = ORIENTED_EDGE ( 'NONE', *, *, #5375, .T. ) ;
#6510 = FACE_OUTER_BOUND ( 'NONE', #11352, .T. ) ;
#6511 = CARTESIAN_POINT ( 'NONE',  ( 52.25172492374522903, 53.59948385550241312, -7.007379884777227730 ) ) ;
#6512 = AXIS2_PLACEMENT_3D ( 'NONE', #10867, #12343, #12438 ) ;
#6513 = VERTEX_POINT ( 'NONE', #555 ) ;
#6514 = DIRECTION ( 'NONE',  ( -0.2439756946365075896, 0.9697813467099857254, 1.610118993450814692E-22 ) ) ;
#6515 = ORIENTED_EDGE ( 'NONE', *, *, #14646, .T. ) ;
#6516 = CARTESIAN_POINT ( 'NONE',  ( 52.62207051974839089, 50.39948385550241738, 7.992620115222770494 ) ) ;
#6517 = DIRECTION ( 'NONE',  ( 0.000000000000000000, -0.000000000000000000, 1.000000000000000000 ) ) ;
#6518 = EDGE_CURVE ( 'NONE', #12905, #9774, #7851, .T. ) ;
#6519 = CARTESIAN_POINT ( 'NONE',  ( 43.33558569842703179, 65.09948385550239891, -2.141517661632099223 ) ) ;
#6520 = CARTESIAN_POINT ( 'NONE',  ( 10.00000000000000000, 20.00000000000001421, 15.00000000000000000 ) ) ;
#6521 = EDGE_CURVE ( 'NONE', #7980, #6445, #9558, .T. ) ;
#6522 = DIRECTION ( 'NONE',  ( 0.9995917534020515305, -0.02857142857142857054, 0.000000000000000000 ) ) ;
#6523 = CARTESIAN_POINT ( 'NONE',  ( 54.13287192849671214, 62.70051614449766220, -5.649768623646139964 ) ) ;
#6524 = DIRECTION ( 'NONE',  ( 0.000000000000000000, 0.000000000000000000, 1.000000000000000000 ) ) ;
#6525 = CARTESIAN_POINT ( 'NONE',  ( 44.03140696652192787, 61.19948385550239323, -4.306917132069425058 ) ) ;
#6526 = CARTESIAN_POINT ( 'NONE',  ( 7.211304515372446211, -1.345319965580511479, 0.000000000000000000 ) ) ;
#6527 = EDGE_LOOP ( 'NONE', ( #13958, #1667, #3186, #2118, #13628 ) ) ;
#6528 = AXIS2_PLACEMENT_3D ( 'NONE', #15950, #8289, #6823 ) ;
#6529 = ORIENTED_EDGE ( 'NONE', *, *, #2526, .T. ) ;
#6530 = DIRECTION ( 'NONE',  ( -1.000000000000000000, -0.000000000000000000, -0.000000000000000000 ) ) ;
#6531 = PRESENTATION_STYLE_ASSIGNMENT (( #17137 ) ) ;
#6532 = CARTESIAN_POINT ( 'NONE',  ( 52.25172492374522903, 51.59948385550240602, -7.007379884777225953 ) ) ;
#6533 = CYLINDRICAL_SURFACE ( 'NONE', #3422, 4.800000000000000711 ) ;
#6534 = STYLED_ITEM ( 'NONE', ( #10460 ), #17389 ) ;
#6535 = ORIENTED_EDGE ( 'NONE', *, *, #6092, .F. ) ;
#6536 = EDGE_LOOP ( 'NONE', ( #11374, #8464, #3586, #180 ) ) ;
#6537 = CARTESIAN_POINT ( 'NONE',  ( -11.75570504584937481, -36.18033988749900942, -9.000000000000000000 ) ) ;
#6538 = VERTEX_POINT ( 'NONE', #13967 ) ;
#6539 = DIRECTION ( 'NONE',  ( 0.000000000000000000, 0.000000000000000000, 1.000000000000000000 ) ) ;
#6540 = ORIENTED_EDGE ( 'NONE', *, *, #13415, .F. ) ;
#6541 = VECTOR ( 'NONE', #13466, 1000.000000000000000 ) ;
#6542 = AXIS2_PLACEMENT_3D ( 'NONE', #3772, #5334, #3867 ) ;
#6543 = CARTESIAN_POINT ( 'NONE',  ( 62.50000000000000000, 32.50000000000001421, 15.00000000000000000 ) ) ;
#6544 = UNCERTAINTY_MEASURE_WITH_UNIT (LENGTH_MEASURE( 1.000000000000000082E-05 ), #7590, 'distance_accuracy_value', 'NONE');
#6545 = CARTESIAN_POINT ( 'NONE',  ( 30.00000000000000000, 3.000000000000000000, -5.999999999999998224 ) ) ;
#6546 = SHAPE_REPRESENTATION ( 'Mounting block', ( #10359 ), #1294 ) ;
#6547 = CARTESIAN_POINT ( 'NONE',  ( 44.30067958973594955, 60.10051614449766788, -1.875703265242155693 ) ) ;
#6548 = CARTESIAN_POINT ( 'NONE',  ( -20.00000000000000000, -25.00000000000000000, -23.00000000000000000 ) ) ;
#6549 = AXIS2_PLACEMENT_3D ( 'NONE', #6969, #5497, #2589 ) ;
#6550 = CARTESIAN_POINT ( 'NONE',  ( 45.15499999999999403, 0.000000000000000000, 0.000000000000000000 ) ) ;
#6551 = CARTESIAN_POINT ( 'NONE',  ( 42.38452918213190657, 57.90051614449765793, 2.450534656007115508 ) ) ;
#6552 = ORIENTED_EDGE ( 'NONE', *, *, #8309, .F. ) ;
#6553 = VERTEX_POINT ( 'NONE', #10652 ) ;
#6554 = CARTESIAN_POINT ( 'NONE',  ( -18.68843350152494054, -12.87662627267948956, 0.000000000000000000 ) ) ;
#6555 = FILL_AREA_STYLE ('',( #17160 ) ) ;
#6556 = CIRCLE ( 'NONE', #6862, 7.000000000000000000 ) ;
#6557 = CARTESIAN_POINT ( 'NONE',  ( 2.000000000000000000, -0.8865213383406730374, -1.535499999999999421 ) ) ;
#6558 = ITEM_DEFINED_TRANSFORMATION ( 'NONE', 'NONE', #297,  #10359 ) ;
#6559 = ORIENTED_EDGE ( 'NONE', *, *, #16885, .T. ) ;
#6560 = FACE_OUTER_BOUND ( 'NONE', #1512, .T. ) ;
#6561 = ADVANCED_FACE ( 'NONE', ( #12123 ), #15262, .F. ) ;
#6562 = FACE_OUTER_BOUND ( 'NONE', #11946, .T. ) ;
#6563 = CIRCLE ( 'NONE', #17547, 3.309499999999999886 ) ;
#6564 = EDGE_LOOP ( 'NONE', ( #8593, #13216, #15455, #16862 ) ) ;
#6565 = EDGE_CURVE ( 'NONE', #6328, #16569, #9186, .T. ) ;
#6566 = CARTESIAN_POINT ( 'NONE',  ( -0.5000000000000000000, -6.429618962271402616, -1.000000000000000000 ) ) ;
#6567 = FACE_OUTER_BOUND ( 'NONE', #4273, .T. ) ;
#6568 = CIRCLE ( 'NONE', #8463, 2.649999999999985700 ) ;
#6569 = DIRECTION ( 'NONE',  ( 0.000000000000000000, -1.000000000000000000, 0.000000000000000000 ) ) ;
#6570 = DIRECTION ( 'NONE',  ( -0.000000000000000000, -0.000000000000000000, 1.000000000000000000 ) ) ;
#6571 = CARTESIAN_POINT ( 'NONE',  ( 42.63976443033212860, 62.99948385550241170, 0.02388180880522514787 ) ) ;
#6572 = CARTESIAN_POINT ( 'NONE',  ( 6.270568613849413886, 4.911887854652841057, 1.704496029161937320 ) ) ;
#6573 = CIRCLE ( 'NONE', #5023, 5.560781378645573980 ) ;
#6574 = CARTESIAN_POINT ( 'NONE',  ( 56.81924384183011512, 60.19948385550240744, 4.924951120819313743 ) ) ;
#6575 = CARTESIAN_POINT ( 'NONE',  ( 54.13287192849671214, 58.70051614449765509, -5.649768623646139964 ) ) ;
#6576 = CIRCLE ( 'NONE', #18499, 20.00000000000000000 ) ;
#6577 = FACE_OUTER_BOUND ( 'NONE', #11225, .T. ) ;
#6578 = CYLINDRICAL_SURFACE ( 'NONE', #14736, 6.080745460913608902 ) ;
#6579 =( NAMED_UNIT ( * ) PLANE_ANGLE_UNIT ( ) SI_UNIT ( $, .RADIAN. ) );
#6580 = VERTEX_POINT ( 'NONE', #15169 ) ;
#6581 = AXIS2_PLACEMENT_3D ( 'NONE', #16986, #15398, #17076 ) ;
#6582 = FILL_AREA_STYLE ('',( #18863 ) ) ;
#6583 = FACE_OUTER_BOUND ( 'NONE', #3018, .T. ) ;
#6584 = AXIS2_PLACEMENT_3D ( 'NONE', #5174, #16772, #15383 ) ;
#6585 = AXIS2_PLACEMENT_3D ( 'NONE', #10419, #11791, #7294 ) ;
#6586 = CARTESIAN_POINT ( 'NONE',  ( 52.29715082351539479, 46.60051614449766078, -6.992620115222796251 ) ) ;
#6587 = CARTESIAN_POINT ( 'NONE',  ( 4.151274195509685683, -2.039912954708743786, 3.533232880573501156 ) ) ;
#6588 = CIRCLE ( 'NONE', #17581, 4.424999999999999822 ) ;
#6589 = CARTESIAN_POINT ( 'NONE',  ( 5.000000000000003553, -20.00000000000000000, 9.000000000000000000 ) ) ;
#6590 = EDGE_LOOP ( 'NONE', ( #9665, #5516, #4486, #13245, #9568 ) ) ;
#6591 = LINE ( 'NONE', #6397, #9587 ) ;
#6592 = DIRECTION ( 'NONE',  ( 0.000000000000000000, 0.000000000000000000, 1.000000000000000000 ) ) ;
#6593 = CARTESIAN_POINT ( 'NONE',  ( 53.54508667620428497, 64.29948385550240175, 4.840751629271157874 ) ) ;
#6594 = CARTESIAN_POINT ( 'NONE',  ( 4.024499207728657879, -2.323545700935587988, -3.572172305156509964 ) ) ;
#6595 = LINE ( 'NONE', #5219, #470 ) ;
#6596 = CARTESIAN_POINT ( 'NONE',  ( 1.000000000000000000, -4.808326913195983821, -0.8000000000000000444 ) ) ;
#6597 = CARTESIAN_POINT ( 'NONE',  ( 52.57664461997821093, 61.40051614449765793, 8.007379884777206414 ) ) ;
#6598 = AXIS2_PLACEMENT_3D ( 'NONE', #7634, #11951, #3 ) ;
#6599 = CARTESIAN_POINT ( 'NONE',  ( 51.92680522751238925, 61.40051614449765793, 6.007379884777208190 ) ) ;
#6600 = CARTESIAN_POINT ( 'NONE',  ( 1.925929944387235853E-31, 15.00000000000001599, 15.00000000000000000 ) ) ;
#6601 = CIRCLE ( 'NONE', #9425, 4.000000000000000000 ) ;
#6602 = PLANE ( 'NONE',  #325 ) ;
#6603 = VERTEX_POINT ( 'NONE', #15362 ) ;
#6604 = ADVANCED_BREP_SHAPE_REPRESENTATION ( '', ( #14915, #10359 ), #12491 ) ;
#6605 = ORIENTED_EDGE ( 'NONE', *, *, #2208, .F. ) ;
#6606 = CARTESIAN_POINT ( 'NONE',  ( 2.449293598294706513E-15, -20.00000000000000000, -9.000000000000000000 ) ) ;
#6607 = VERTEX_POINT ( 'NONE', #3506 ) ;
#6608 = EDGE_CURVE ( 'NONE', #9923, #13221, #2036, .T. ) ;
#6609 = CARTESIAN_POINT ( 'NONE',  ( -150.9999999999999432, -14.99999999999999645, -15.00000000000000000 ) ) ;
#6610 = ORIENTED_EDGE ( 'NONE', *, *, #8951, .F. ) ;
#6611 = LINE ( 'NONE', #10734, #5642 ) ;
#6612 = PRODUCT_DEFINITION ( 'UNKNOWN', '', #16072, #14991 ) ;
#6613 = CARTESIAN_POINT ( 'NONE',  ( 44.03140696652193498, 53.19948385550240033, -4.306917132069424170 ) ) ;
#6614 = ORIENTED_EDGE ( 'NONE', *, *, #1606, .F. ) ;
#6615 = CARTESIAN_POINT ( 'NONE',  ( 6.452281807715810835, -2.898928808472999830, -5.021091983800332947 ) ) ;
#6616 = CIRCLE ( 'NONE', #3196, 5.000000000000000888 ) ;
#6617 = ORIENTED_EDGE ( 'NONE', *, *, #15872, .T. ) ;
#6618 = CARTESIAN_POINT ( 'NONE',  ( 54.68390685589033495, 53.69948385550240744, -6.485486291978119766 ) ) ;
#6619 = AXIS2_PLACEMENT_3D ( 'NONE', #9033, #17982, #7472 ) ;
#6620 = LINE ( 'NONE', #14156, #10755 ) ;
#6621 = CARTESIAN_POINT ( 'NONE',  ( 55.94051828345050836, 61.79948385550239465, -4.345558710429104465 ) ) ;
#6622 = CARTESIAN_POINT ( 'NONE',  ( -74.99999999999997158, -1.000000000000000000, 6.000000000000001776 ) ) ;
#6623 = CIRCLE ( 'NONE', #11630, 4.799999999999999822 ) ;
#6624 = LINE ( 'NONE', #14257, #10561 ) ;
#6625 = CARTESIAN_POINT ( 'NONE',  ( 47.74827507625469281, 60.40051614449767214, -7.007379884777203749 ) ) ;
#6626 = EDGE_CURVE ( 'NONE', #3807, #6955, #1747, .T. ) ;
#6627 = CARTESIAN_POINT ( 'NONE',  ( 44.03140696652192787, 57.19948385550238612, -4.306917132069425058 ) ) ;
#6628 = CARTESIAN_POINT ( 'NONE',  ( -6.473970235329672780E-16, -4.862606272033106691, -3.745885042887442395 ) ) ;
#6629 = CARTESIAN_POINT ( 'NONE',  ( 6.196878017913832970, -3.367876570272822168, -4.166666666666666963 ) ) ;
#6630 = VERTEX_POINT ( 'NONE', #15454 ) ;
#6631 = ORIENTED_EDGE ( 'NONE', *, *, #12754, .T. ) ;
#6632 = DIRECTION ( 'NONE',  ( 0.000000000000000000, 0.000000000000000000, -1.000000000000000000 ) ) ;
#6633 = EDGE_CURVE ( 'NONE', #17604, #13178, #7995, .T. ) ;
#6634 = CARTESIAN_POINT ( 'NONE',  ( 44.05948171654949874, 52.79948385550240175, 4.345558710429105354 ) ) ;
#6635 = VECTOR ( 'NONE', #12020, 1000.000000000000000 ) ;
#6636 = EDGE_CURVE ( 'NONE', #5403, #10751, #18481, .T. ) ;
#6637 = DIRECTION ( 'NONE',  ( -0.000000000000000000, -0.000000000000000000, -1.000000000000000000 ) ) ;
#6638 = ORIENTED_EDGE ( 'NONE', *, *, #10234, .T. ) ;
#6639 = ORIENTED_EDGE ( 'NONE', *, *, #787, .F. ) ;
#6640 = DIRECTION ( 'NONE',  ( -0.9993267699245929059, -0.03668796685672145313, -2.853726094247056096E-17 ) ) ;
#6641 = VERTEX_POINT ( 'NONE', #9945 ) ;
#6642 = CARTESIAN_POINT ( 'NONE',  ( 50.02271294988505446, 64.50051614449765225, -7.000000000000000888 ) ) ;
#6643 = VERTEX_POINT ( 'NONE', #5355 ) ;
#6644 = EDGE_CURVE ( 'NONE', #8664, #3916, #14707, .T. ) ;
#6645 = DIRECTION ( 'NONE',  ( -1.000000000000000000, 1.110223024625156935E-15, 0.000000000000000000 ) ) ;
#6646 = B_SPLINE_CURVE_WITH_KNOTS ( 'NONE', 3,
 ( #8577, #5433, #14743, #11411, #18990, #17415 ),
 .UNSPECIFIED., .F., .F.,
 ( 4, 2, 4 ),
 ( 0.002044882221487534079, 0.003063384235218496315, 0.004081886248949458985 ),
 .UNSPECIFIED. ) ;
#6647 = DIRECTION ( 'NONE',  ( -0.000000000000000000, -0.000000000000000000, 1.000000000000000000 ) ) ;
#6648 = VECTOR ( 'NONE', #13279, 1000.000000000000000 ) ;
#6649 = CARTESIAN_POINT ( 'NONE',  ( 44.30067958973594955, 62.10051614449765367, -1.875703265242155693 ) ) ;
#6650 = CARTESIAN_POINT ( 'NONE',  ( 7.211304515372821022, -38.65468003441933575, 9.000000000000000000 ) ) ;
#6651 = DIRECTION ( 'NONE',  ( -1.000000000000000000, 0.000000000000000000, 0.000000000000000000 ) ) ;
#6652 = DIRECTION ( 'NONE',  ( 0.000000000000000000, -0.000000000000000000, 1.000000000000000000 ) ) ;
#6653 =( REPRESENTATION_RELATIONSHIP ('NONE','NONE', #16703, #14681 ) REPRESENTATION_RELATIONSHIP_WITH_TRANSFORMATION ( #14099 )SHAPE_REPRESENTATION_RELATIONSHIP( ) );
#6654 = CARTESIAN_POINT ( 'NONE',  ( 54.68390685589039890, 57.30051614449767072, 6.485486291978072693 ) ) ;
#6655 = ORIENTED_EDGE ( 'NONE', *, *, #6993, .T. ) ;
#6656 = ORIENTED_EDGE ( 'NONE', *, *, #16120, .F. ) ;
#6657 = CYLINDRICAL_SURFACE ( 'NONE', #15285, 20.00000000000000000 ) ;
#6658 = EDGE_CURVE ( 'NONE', #6708, #9457, #13797, .T. ) ;
#6659 = DIRECTION ( 'NONE',  ( -0.000000000000000000, -0.000000000000000000, 1.000000000000000000 ) ) ;
#6660 = ITEM_DEFINED_TRANSFORMATION ( 'NONE', 'NONE', #12924,  #10359 ) ;
#6661 = ORIENTED_EDGE ( 'NONE', *, *, #6879, .T. ) ;
#6662 = DIRECTION ( 'NONE',  ( -0.000000000000000000, -0.000000000000000000, -1.000000000000000000 ) ) ;
#6663 = CARTESIAN_POINT ( 'NONE',  ( -14.17539641854921229, -5.891203581560112923, 0.000000000000000000 ) ) ;
#6664 = VERTEX_POINT ( 'NONE', #746 ) ;
#6665 = AXIS2_PLACEMENT_3D ( 'NONE', #13334, #8835, #11861 ) ;
#6666 = CARTESIAN_POINT ( 'NONE',  ( 30.00000000000000355, -40.00000000000000000, 10.00000000000000000 ) ) ;
#6667 = DIRECTION ( 'NONE',  ( 1.000000000000000000, 0.000000000000000000, 0.000000000000000000 ) ) ;
#6668 = FACE_BOUND ( 'NONE', #6130, .T. ) ;
#6669 = CARTESIAN_POINT ( 'NONE',  ( 2.000000000000000000, -1.329782007511005837, 0.7677500000000023750 ) ) ;
#6670 = DIRECTION ( 'NONE',  ( -0.000000000000000000, -0.000000000000000000, -1.000000000000000000 ) ) ;
#6671 = CARTESIAN_POINT ( 'NONE',  ( 49.97728705011488159, 63.49948385550241170, -7.000000000000000888 ) ) ;
#6672 = CARTESIAN_POINT ( 'NONE',  ( 1.567478505476134606E-15, 4.618802153517012066, -5.000000000000000000 ) ) ;
#6673 = CARTESIAN_POINT ( 'NONE',  ( 54.72065718078924590, 58.29948385550240886, 6.458785618021043895 ) ) ;
#6674 = CARTESIAN_POINT ( 'NONE',  ( 44.03140696652198471, 63.80051614449765651, 4.306917132069485454 ) ) ;
#6675 = EDGE_CURVE ( 'NONE', #10827, #7050, #12604, .T. ) ;
#6676 = DIRECTION ( 'NONE',  ( -1.000000000000000000, 0.000000000000000000, 0.000000000000000000 ) ) ;
#6677 =( NAMED_UNIT ( * ) SI_UNIT ( $, .STERADIAN. ) SOLID_ANGLE_UNIT ( ) );
#6678 = ADVANCED_FACE ( 'NONE', ( #6720 ), #349, .T. ) ;
#6679 = DIRECTION ( 'NONE',  ( 0.000000000000000000, 0.000000000000000000, 1.000000000000000000 ) ) ;
#6680 = VERTEX_POINT ( 'NONE', #11328 ) ;
#6681 = CARTESIAN_POINT ( 'NONE',  ( 32.00000000000000000, 1.000000000000000000, 6.000000000000000000 ) ) ;
#6682 = DIRECTION ( 'NONE',  ( 0.000000000000000000, 0.000000000000000000, 1.000000000000000000 ) ) ;
#6683 = CARTESIAN_POINT ( 'NONE',  ( 44.05948171654945611, 54.20051614449765509, -4.345558710429044069 ) ) ;
#6684 = CARTESIAN_POINT ( 'NONE',  ( 2.449293598294706513E-15, -20.00000000000000000, 9.000000000000000000 ) ) ;
#6685 = LINE ( 'NONE', #4927, #14612 ) ;
#6686 = ORIENTED_EDGE ( 'NONE', *, *, #11299, .T. ) ;
#6687 = FACE_OUTER_BOUND ( 'NONE', #15827, .T. ) ;
#6688 = CARTESIAN_POINT ( 'NONE',  ( 30.00000000000000355, 0.000000000000000000, -10.00000000000000000 ) ) ;
#6689 = CARTESIAN_POINT ( 'NONE',  ( 0.000000000000000000, 0.000000000000000000, -1.000000000000000000 ) ) ;
#6690 =( NAMED_UNIT ( * ) PLANE_ANGLE_UNIT ( ) SI_UNIT ( $, .RADIAN. ) );
#6691 = FACE_BOUND ( 'NONE', #6831, .T. ) ;
#6692 = CARTESIAN_POINT ( 'NONE',  ( 50.02271294988505446, 58.50051614449765225, -8.000000000000001776 ) ) ;
#6693 = CARTESIAN_POINT ( 'NONE',  ( 44.30067958973594955, 60.10051614449766788, -1.875703265242155693 ) ) ;
#6694 = EDGE_CURVE ( 'NONE', #5258, #1202, #691, .T. ) ;
#6695 = AXIS2_PLACEMENT_3D ( 'NONE', #10041, #14354, #8765 ) ;
#6696 = DIRECTION ( 'NONE',  ( -0.000000000000000000, -0.000000000000000000, 1.000000000000000000 ) ) ;
#6697 = CARTESIAN_POINT ( 'NONE',  ( 4.175813232069146785, 2.061359961916365613, -3.570380186727397653 ) ) ;
#6698 = AXIS2_PLACEMENT_3D ( 'NONE', #11982, #17647, #1550 ) ;
#6699 = VERTEX_POINT ( 'NONE', #17330 ) ;
#6700 = EDGE_LOOP ( 'NONE', ( #16148, #12706, #18939, #5183 ) ) ;
#6701 = EDGE_LOOP ( 'NONE', ( #13366, #5549, #14200, #4093 ) ) ;
#6702 = DIRECTION ( 'NONE',  ( 1.000000000000000000, 1.387778780781445676E-16, 0.000000000000000000 ) ) ;
#6703 = ORIENTED_EDGE ( 'NONE', *, *, #3650, .T. ) ;
#6704 = DIRECTION ( 'NONE',  ( 1.000000000000000000, -0.000000000000000000, -0.000000000000000000 ) ) ;
#6705 = EDGE_LOOP ( 'NONE', ( #6656, #19117, #12616, #5163 ) ) ;
#6706 = CARTESIAN_POINT ( 'NONE',  ( 2.449293598294706513E-15, -20.00000000000000000, -9.000000000000000000 ) ) ;
#6707 = CARTESIAN_POINT ( 'NONE',  ( 47.70284917648453415, 57.39948385550240317, -6.992620115222774047 ) ) ;
#6708 = VERTEX_POINT ( 'NONE', #946 ) ;
#6709 = CARTESIAN_POINT ( 'NONE',  ( -20.00000000000000000, -19.99999999999999289, -23.00000000000000000 ) ) ;
#6710 = EDGE_LOOP ( 'NONE', ( #9354, #8522, #17657, #4854 ) ) ;
#6711 = CARTESIAN_POINT ( 'NONE',  ( 45.31609314410967926, 54.69948385550240033, 6.485486291978119766 ) ) ;
#6712 = VECTOR ( 'NONE', #8532, 1000.000000000000114 ) ;
#6713 = DIRECTION ( 'NONE',  ( 0.000000000000000000, 0.000000000000000000, 1.000000000000000000 ) ) ;
#6714 = CARTESIAN_POINT ( 'NONE',  ( 47.70284917648453415, 61.39948385550241738, -6.992620115222774047 ) ) ;
#6715 = CARTESIAN_POINT ( 'NONE',  ( 4.158806965674306078, 1.986429158307092768, 3.559403772175832259 ) ) ;
#6716 = LINE ( 'NONE', #5247, #3687 ) ;
#6717 = CARTESIAN_POINT ( 'NONE',  ( 56.65037692655921120, 59.10051614449766078, 2.184720259617097593 ) ) ;
#6718 = CARTESIAN_POINT ( 'NONE',  ( 44.91013252490152752, 60.79948385550241596, 3.727524721679198461 ) ) ;
#6719 = CARTESIAN_POINT ( 'NONE',  ( 52.29715082351547295, 56.39948385550238896, 6.992620115222774047 ) ) ;
#6720 = FACE_OUTER_BOUND ( 'NONE', #13180, .T. ) ;
#6721 = DIRECTION ( 'NONE',  ( -0.7779254092217071648, -0.6283566325640553840, 0.000000000000000000 ) ) ;
#6722 = ORIENTED_EDGE ( 'NONE', *, *, #13988, .F. ) ;
#6723 = AXIS2_PLACEMENT_3D ( 'NONE', #11262, #15696, #7053 ) ;
#6724 = VERTEX_POINT ( 'NONE', #3889 ) ;
#6725 = CARTESIAN_POINT ( 'NONE',  ( 11.75570504584960041, -36.18033988749885310, -9.000000000000000000 ) ) ;
#6726 = AXIS2_PLACEMENT_3D ( 'NONE', #2355, #9872, #2652 ) ;
#6727 = CARTESIAN_POINT ( 'NONE',  ( 55.94051828345050836, 59.79948385550238754, -4.345558710429104465 ) ) ;
#6728 = DIRECTION ( 'NONE',  ( -0.7779254092217071648, -0.6283566325640553840, 0.000000000000000000 ) ) ;
#6729 = EDGE_LOOP ( 'NONE', ( #7611, #4099, #14653, #11149 ) ) ;
#6730 = ORIENTED_EDGE ( 'NONE', *, *, #5075, .T. ) ;
#6731 = CARTESIAN_POINT ( 'NONE',  ( 0.000000000000000000, 0.000000000000000000, 0.000000000000000000 ) ) ;
#6732 = EDGE_LOOP ( 'NONE', ( #9830, #7041, #13953, #13790 ) ) ;
#6733 = FACE_OUTER_BOUND ( 'NONE', #10350, .T. ) ;
#6734 = ORIENTED_EDGE ( 'NONE', *, *, #11665, .T. ) ;
#6735 = CARTESIAN_POINT ( 'NONE',  ( 43.34962307344081012, 46.89948385550240317, 2.184720259617164650 ) ) ;
#6736 = DIRECTION ( 'NONE',  ( -0.000000000000000000, 0.000000000000000000, 1.000000000000000000 ) ) ;
#6737 = CARTESIAN_POINT ( 'NONE',  ( 56.30877334542961421, 59.00051614449766646, 0.02388180880515774693 ) ) ;
#6738 = DIRECTION ( 'NONE',  ( -0.000000000000000000, -0.000000000000000000, -1.000000000000000000 ) ) ;
#6739 = ADVANCED_FACE ( 'NONE', ( #12704 ), #11919, .T. ) ;
#6740 = CARTESIAN_POINT ( 'NONE',  ( 2.449293598294706513E-15, -20.00000000000000000, -10.00000000000000000 ) ) ;
#6741 = CARTESIAN_POINT ( 'NONE',  ( 19.97007065299861139, -18.90625500492856759, 0.000000000000000000 ) ) ;
#6742 = PRODUCT_DEFINITION ( 'UNKNOWN', '', #2301, #18539 ) ;
#6743 = AXIS2_PLACEMENT_3D ( 'NONE', #14912, #12349, #14002 ) ;
#6744 = ADVANCED_FACE ( 'NONE', ( #15753 ), #6918, .T. ) ;
#6745 = ORIENTED_EDGE ( 'NONE', *, *, #19262, .T. ) ;
#6746 = EDGE_LOOP ( 'NONE', ( #17438, #14375 ) ) ;
#6747 = CARTESIAN_POINT ( 'NONE',  ( 4.211399257449709665, -2.459727064652517114, -3.751161691472417736 ) ) ;
#6748 = EDGE_CURVE ( 'NONE', #206, #15249, #2430, .T. ) ;
#6749 = EDGE_CURVE ( 'NONE', #9866, #1761, #1288, .T. ) ;
#6750=STYLED_ITEM('',(#19475),#2292);
#6751 = FILL_AREA_STYLE_COLOUR ( '', #5583 ) ;
#6752 = ORIENTED_EDGE ( 'NONE', *, *, #1197, .F. ) ;
#6753 = CARTESIAN_POINT ( 'NONE',  ( 2.449293598294706513E-15, -20.00000000000000000, -9.000000000000000000 ) ) ;
#6754 = EDGE_CURVE ( 'NONE', #12106, #4903, #5443, .T. ) ;
#6755 = DIRECTION ( 'NONE',  ( 1.000000000000000000, 0.000000000000000000, 0.000000000000000000 ) ) ;
#6756 = ORIENTED_EDGE ( 'NONE', *, *, #10945, .F. ) ;
#6757 = AXIS2_PLACEMENT_3D ( 'NONE', #17436, #17725, #12817 ) ;
#6758 = DIRECTION ( 'NONE',  ( -0.000000000000000000, -0.000000000000000000, 1.000000000000000000 ) ) ;
#6759 = CARTESIAN_POINT ( 'NONE',  ( -2.354826896168714434, -6.962563485461402024, -1.000000000000000000 ) ) ;
#6760 = FACE_OUTER_BOUND ( 'NONE', #11036, .T. ) ;
#6761 = CARTESIAN_POINT ( 'NONE',  ( -74.99999999999997158, 40.00000000000001421, 10.00000000000000000 ) ) ;
#6762 = PRODUCT_DEFINITION_SHAPE ( 'NONE', 'NONE',  #3046 ) ;
#6763 = EDGE_CURVE ( 'NONE', #4747, #6937, #9412, .T. ) ;
#6764 = CARTESIAN_POINT ( 'NONE',  ( 0.000000000000000000, 3.755786496842903495E-16, 3.500000000000000000 ) ) ;
#6765 = CIRCLE ( 'NONE', #824, 8.000000000000007105 ) ;
#6766 = ADVANCED_FACE ( 'NONE', ( #60 ), #17714, .T. ) ;
#6767 = CARTESIAN_POINT ( 'NONE',  ( 44.03140696652192787, 65.19948385550240744, -4.306917132069425058 ) ) ;
#6768 = DIRECTION ( 'NONE',  ( 1.000000000000000000, 0.000000000000000000, 0.000000000000000000 ) ) ;
#6769 = CARTESIAN_POINT ( 'NONE',  ( 54.72065718078924590, 64.29948385550240175, 6.458785618021043895 ) ) ;
#6770 = CARTESIAN_POINT ( 'NONE',  ( 47.70284917648459100, 61.60051614449764656, 6.992620115222796251 ) ) ;
#6771 = CARTESIAN_POINT ( 'NONE',  ( -164.9999999999999716, -14.99999999999999645, 4.000000000000000000 ) ) ;
#6772 = CARTESIAN_POINT ( 'NONE',  ( 6.506891779418572774, 5.826362946429627598, 0.09155664655281574305 ) ) ;
#6773 = CONICAL_SURFACE ( 'NONE', #4906, 5.560781378645573980, 1.221730476396046816 ) ;
#6774 =( NAMED_UNIT ( * ) PLANE_ANGLE_UNIT ( ) SI_UNIT ( $, .RADIAN. ) );
#6775 = ORIENTED_EDGE ( 'NONE', *, *, #2841, .T. ) ;
#6776 = CARTESIAN_POINT ( 'NONE',  ( -22.00000000000000000, -19.99999999999999289, -12.00000000000000000 ) ) ;
#6777 = PRODUCT_DEFINITION_SHAPE ( 'NONE', 'NONE',  #19432 ) ;
#6778 = PLANE ( 'NONE',  #8756 ) ;
#6779 = CARTESIAN_POINT ( 'NONE',  ( 45.90387839640208512, 52.30051614449766362, -5.676469297603124353 ) ) ;
#6780 = AXIS2_PLACEMENT_3D ( 'NONE', #5027, #3470, #1998 ) ;
#6781 = DIRECTION ( 'NONE',  ( -0.6691306063588624564, 0.7431448254773903583, 0.000000000000000000 ) ) ;
#6782 = CARTESIAN_POINT ( 'NONE',  ( 2.449293598294706513E-15, -20.00000000000000000, -9.000000000000000000 ) ) ;
#6783 = EDGE_LOOP ( 'NONE', ( #6752, #4722, #6992, #14669 ) ) ;
#6784 = DIRECTION ( 'NONE',  ( 1.000000000000000000, 0.000000000000000000, 0.000000000000000000 ) ) ;
#6785 = AXIS2_PLACEMENT_3D ( 'NONE', #4102, #5663, #4393 ) ;
#6786 = DIRECTION ( 'NONE',  ( -0.02045300604585054485, -0.9997908153927442809, -2.853726094247055479E-17 ) ) ;
#6787 = CARTESIAN_POINT ( 'NONE',  ( -5.686050877451574337, -5.768780236673276995, -1.000000000000000000 ) ) ;
#6788 = DIRECTION ( 'NONE',  ( -0.4999999999999933942, -0.8660254037844425934, 0.000000000000000000 ) ) ;
#6789 = CARTESIAN_POINT ( 'NONE',  ( 45.27934281921075410, 47.29948385550241596, -6.458785618021043895 ) ) ;
#6790 = CARTESIAN_POINT ( 'NONE',  ( 43.69122665457040000, 64.00051614449765225, -0.02388180880515696977 ) ) ;
#6791 = CLOSED_SHELL ( 'NONE', ( #8240, #10768, #2347, #7363, #11435, #10168, #15494, #14396, #12169, #17554, #8540, #3569, #18761, #512, #4363, #3188, #17086, #8563, #15078, #9604, #17238, #410, #3116, #9169, #5845, #6408, #13465, #2759, #1387, #522, #11583, #17549 ) ) ;
#6792 = DIRECTION ( 'NONE',  ( 0.000000000000000000, 0.000000000000000000, 1.000000000000000000 ) ) ;
#6793 = CARTESIAN_POINT ( 'NONE',  ( 6.541334450618642826, 2.987059910623326875, 5.112749838330405083 ) ) ;
#6794 = EDGE_LOOP ( 'NONE', ( #8575, #4159, #9475, #4346 ) ) ;
#6795 = VERTEX_POINT ( 'NONE', #7207 ) ;
#6796 = VERTEX_POINT ( 'NONE', #3104 ) ;
#6797 = DIRECTION ( 'NONE',  ( -0.8660254037844377084, -0.5000000000000015543, 0.000000000000000000 ) ) ;
#6798 = AXIS2_PLACEMENT_3D ( 'NONE', #2627, #7305, #14746 ) ;
#6799 = VERTEX_POINT ( 'NONE', #8963 ) ;
#6800 = CARTESIAN_POINT ( 'NONE',  ( 3.950250160040163383, -0.7258013381021514165, 3.499999999999845013 ) ) ;
#6801 = EDGE_LOOP ( 'NONE', ( #11716, #6756, #12178, #7577 ) ) ;
#6802 = FACE_OUTER_BOUND ( 'NONE', #7792, .T. ) ;
#6803 = CARTESIAN_POINT ( 'NONE',  ( 49.97728705011488159, 59.49948385550240459, -7.000000000000000888 ) ) ;
#6804 = EDGE_CURVE ( 'NONE', #18672, #762, #8384, .T. ) ;
#6805 = ORIENTED_EDGE ( 'NONE', *, *, #9511, .T. ) ;
#6806 = DIRECTION ( 'NONE',  ( 1.000000000000000000, 0.000000000000000000, 0.000000000000000000 ) ) ;
#6807 = ORIENTED_EDGE ( 'NONE', *, *, #15756, .T. ) ;
#6808 = CIRCLE ( 'NONE', #11176, 20.00000000000000000 ) ;
#6809 = CARTESIAN_POINT ( 'NONE',  ( 49.97728705011486738, 55.49948385550241170, -8.000000000000001776 ) ) ;
#6810 = CARTESIAN_POINT ( 'NONE',  ( 3.950233766685291137, 0.7256672287179410930, -3.499999999999844125 ) ) ;
#6811 = EDGE_CURVE ( 'NONE', #7334, #4677, #15698, .T. ) ;
#6812 = AXIS2_PLACEMENT_3D ( 'NONE', #15705, #10101, #5495 ) ;
#6813 = CARTESIAN_POINT ( 'NONE',  ( 55.11794222512601493, 50.19948385550241454, 3.688883143319541702 ) ) ;
#6814 = CARTESIAN_POINT ( 'NONE',  ( 4.165266963751723672, 2.049631966911992009, -3.550066703508905963 ) ) ;
#6815 = PLANE ( 'NONE',  #4306 ) ;
#6816 = VECTOR ( 'NONE', #4267, 1000.000000000000000 ) ;
#6817 = CARTESIAN_POINT ( 'NONE',  ( 50.02271294988505446, 62.50051614449766646, -7.000000000000000888 ) ) ;
#6818 = CARTESIAN_POINT ( 'NONE',  ( 55.08986747509847248, 61.79948385550240175, -3.727524721679197572 ) ) ;
#6819 = DIRECTION ( 'NONE',  ( -0.000000000000000000, -0.000000000000000000, -1.000000000000000000 ) ) ;
#6820 = CARTESIAN_POINT ( 'NONE',  ( 5.130877905917027526, -0.6693483836014320065, 0.000000000000000000 ) ) ;
#6821 = ORIENTED_EDGE ( 'NONE', *, *, #2586, .T. ) ;
#6822 = ORIENTED_EDGE ( 'NONE', *, *, #19157, .T. ) ;
#6823 = DIRECTION ( 'NONE',  ( 0.000000000000000000, 1.224646799147351975E-16, 1.000000000000000000 ) ) ;
#6824 = EDGE_LOOP ( 'NONE', ( #10730, #11912, #6486, #4668, #2796 ) ) ;
#6825 = VECTOR ( 'NONE', #14, 1000.000000000000000 ) ;
#6826 = CARTESIAN_POINT ( 'NONE',  ( 55.96859303347804371, 60.19948385550240744, 4.306917132069425946 ) ) ;
#6827 = CARTESIAN_POINT ( 'NONE',  ( -18.68843350152489080, -27.12337372732064011, 9.000000000000000000 ) ) ;
#6828 = EDGE_LOOP ( 'NONE', ( #12442, #8763, #2919, #2727, #16425 ) ) ;
#6829 = ORIENTED_EDGE ( 'NONE', *, *, #670, .F. ) ;
#6830 = LINE ( 'NONE', #3995, #10825 ) ;
#6831 = EDGE_LOOP ( 'NONE', ( #15973, #4252 ) ) ;
#6832 =( GEOMETRIC_REPRESENTATION_CONTEXT ( 3 ) GLOBAL_UNCERTAINTY_ASSIGNED_CONTEXT ( ( #1467 ) ) GLOBAL_UNIT_ASSIGNED_CONTEXT ( ( #8121, #18933, #12637 ) ) REPRESENTATION_CONTEXT ( 'NONE', 'WORKASPACE' ) );
#6833 = LINE ( 'NONE', #4890, #17589 ) ;
#6834 = ORIENTED_EDGE ( 'NONE', *, *, #19015, .T. ) ;
#6835 = CARTESIAN_POINT ( 'NONE',  ( 45.90387839640214196, 48.69948385550240744, 5.676469297603166098 ) ) ;
#6836 = DIRECTION ( 'NONE',  ( 0.000000000000000000, 0.000000000000000000, -1.000000000000000000 ) ) ;
#6837 = CARTESIAN_POINT ( 'NONE',  ( 55.11794222512599362, 58.80051614449766362, -3.688883143319583446 ) ) ;
#6838 = DIRECTION ( 'NONE',  ( -1.000000000000000000, 0.000000000000000000, 0.000000000000000000 ) ) ;
#6839 = CIRCLE ( 'NONE', #17820, 2.649999999999988365 ) ;
#6840 = DIRECTION ( 'NONE',  ( 0.000000000000000000, 0.000000000000000000, -1.000000000000000000 ) ) ;
#6841 = DIRECTION ( 'NONE',  ( -0.000000000000000000, -0.000000000000000000, 1.000000000000000000 ) ) ;
#6842 = EDGE_LOOP ( 'NONE', ( #14973, #7927 ) ) ;
#6843 = VERTEX_POINT ( 'NONE', #14947 ) ;
#6844 = CARTESIAN_POINT ( 'NONE',  ( 4.203935335434060505, 1.640780671294165272, -3.598452447879202598 ) ) ;
#6845 = FILL_AREA_STYLE ('',( #3620 ) ) ;
#6846 = DIRECTION ( 'NONE',  ( -0.000000000000000000, -0.000000000000000000, 1.000000000000000000 ) ) ;
#6847 = DIRECTION ( 'NONE',  ( -1.000000000000000000, 0.000000000000000000, 0.000000000000000000 ) ) ;
#6848 = EDGE_LOOP ( 'NONE', ( #12257, #7527, #15829, #13603 ) ) ;
#6849 = CARTESIAN_POINT ( 'NONE',  ( -62.49999999999997158, 32.50000000000001421, 15.00000000000000000 ) ) ;
#6850 = CIRCLE ( 'NONE', #11538, 1.000000000000000444 ) ;
#6851 = EDGE_CURVE ( 'NONE', #18532, #16520, #1612, .T. ) ;
#6852 = ORIENTED_EDGE ( 'NONE', *, *, #12523, .T. ) ;
#6853 = DIRECTION ( 'NONE',  ( -1.000000000000000000, -0.000000000000000000, 0.000000000000000000 ) ) ;
#6854 = CARTESIAN_POINT ( 'NONE',  ( 4.175326769692857987, 4.121399112977855772, 3.964526709274768569E-16 ) ) ;
#6855 = DIRECTION ( 'NONE',  ( 0.000000000000000000, 0.000000000000000000, 1.000000000000000000 ) ) ;
#6856 = CARTESIAN_POINT ( 'NONE',  ( 1.677125235563514178E-16, 0.3423821193476823121, 3.500000000000000444 ) ) ;
#6857 = CARTESIAN_POINT ( 'NONE',  ( 55.71335778527780747, 48.09948385550240602, 1.832500667257165983 ) ) ;
#6858 = CARTESIAN_POINT ( 'NONE',  ( -9.999999999999994671, 20.00000000000001421, 15.00000000000000000 ) ) ;
#6859 = CARTESIAN_POINT ( 'NONE',  ( 56.65037692655918988, 47.89948385550240317, -2.184720259617163762 ) ) ;
#6860 = AXIS2_PLACEMENT_3D ( 'NONE', #14836, #4457, #14735 ) ;
#6861 = CARTESIAN_POINT ( 'NONE',  ( 42.38452918213190657, 49.90051614449766504, 2.450534656007115508 ) ) ;
#6862 = AXIS2_PLACEMENT_3D ( 'NONE', #13359, #19381, #17893 ) ;
#6863 = ADVANCED_FACE ( 'NONE', ( #11707 ), #6308, .F. ) ;
#6864 = FACE_OUTER_BOUND ( 'NONE', #3216, .T. ) ;
#6865 = CARTESIAN_POINT ( 'NONE',  ( 6.245824673233021151, 4.939548505212935758, -1.655093584846096366 ) ) ;
#6866 = DIRECTION ( 'NONE',  ( 0.9237280213470682178, 0.3830490080632377725, 0.000000000000000000 ) ) ;
#6867 = VERTEX_POINT ( 'NONE', #18007 ) ;
#6868 = DIRECTION ( 'NONE',  ( 1.000000000000000000, 0.000000000000000000, 0.000000000000000000 ) ) ;
#6869 = EDGE_CURVE ( 'NONE', #9645, #15764, #1335, .T. ) ;
#6870 = EDGE_CURVE ( 'NONE', #11790, #9875, #18226, .T. ) ;
#6871 = FACE_OUTER_BOUND ( 'NONE', #19005, .T. ) ;
#6872 = CARTESIAN_POINT ( 'NONE',  ( 56.66441430157294690, 52.90051614449765793, -2.141517661632166281 ) ) ;
#6873 = CIRCLE ( 'NONE', #18803, 20.00000000000000000 ) ;
#6874 = DIRECTION ( 'NONE',  ( 0.000000000000000000, 0.000000000000000000, 1.000000000000000000 ) ) ;
#6875 = CYLINDRICAL_SURFACE ( 'NONE', #3363, 20.00000000000000000 ) ;
#6876 = EDGE_LOOP ( 'NONE', ( #5582, #10088 ) ) ;
#6877 = CARTESIAN_POINT ( 'NONE',  ( -1.149999999999998135, 0.000000000000000000, -4.100000000000000533 ) ) ;
#6878 = DIRECTION ( 'NONE',  ( -0.000000000000000000, -0.000000000000000000, -1.000000000000000000 ) ) ;
#6879 = EDGE_CURVE ( 'NONE', #1029, #3823, #16009, .T. ) ;
#6880 = CARTESIAN_POINT ( 'NONE',  ( -154.9999999999999716, -14.99999999999999645, -15.79999999999999538 ) ) ;
#6881 = CARTESIAN_POINT ( 'NONE',  ( 44.03140696652192787, 51.19948385550238612, -4.306917132069425058 ) ) ;
#6882 = VECTOR ( 'NONE', #4272, 1000.000000000000000 ) ;
#6883 = EDGE_CURVE ( 'NONE', #11986, #4950, #9731, .T. ) ;
#6884 = B_SPLINE_CURVE_WITH_KNOTS ( 'NONE', 3,
 ( #16188, #14508, #14804, #17666, #1383 ),
 .UNSPECIFIED., .F., .F.,
 ( 4, 1, 4 ),
 ( 0.000000000000000000, 0.002309401076758505356, 0.004618802153517010713 ),
 .UNSPECIFIED. ) ;
#6885 = LINE ( 'NONE', #4054, #5441 ) ;
#6886 = CARTESIAN_POINT ( 'NONE',  ( 56.81924384183011512, 46.19948385550240744, 4.924951120819313743 ) ) ;
#6887 = LINE ( 'NONE', #3957, #14764 ) ;
#6888 = CARTESIAN_POINT ( 'NONE',  ( 51.92680522751238925, 59.40051614449765793, 6.007379884777208190 ) ) ;
#6889 = ADVANCED_FACE ( 'NONE', ( #1138 ), #6038, .F. ) ;
#6890 = CARTESIAN_POINT ( 'NONE',  ( -1.000000000000000000, -5.408326913195983465, -0.8000000000000000444 ) ) ;
#6891 = LINE ( 'NONE', #12879, #18829 ) ;
#6892 = CIRCLE ( 'NONE', #12213, 0.5999999999999998668 ) ;
#6893 = ORIENTED_EDGE ( 'NONE', *, *, #1614, .T. ) ;
#6894 = AXIS2_PLACEMENT_3D ( 'NONE', #7415, #13392, #10248 ) ;
#6895 = VERTEX_POINT ( 'NONE', #7404 ) ;
#6896 = CARTESIAN_POINT ( 'NONE',  ( -74.99999999999997158, -23.00000000000000355, 15.00000000000000000 ) ) ;
#6897 = ORIENTED_EDGE ( 'NONE', *, *, #8320, .F. ) ;
#6898 = CARTESIAN_POINT ( 'NONE',  ( -4.000000000000000000, 0.000000000000000000, 0.000000000000000000 ) ) ;
#6899 = AXIS2_PLACEMENT_3D ( 'NONE', #16212, #8943, #3083 ) ;
#6900 = ORIENTED_EDGE ( 'NONE', *, *, #15393, .F. ) ;
#6901 = PLANE ( 'NONE',  #16633 ) ;
#6902 = CARTESIAN_POINT ( 'NONE',  ( 42.63976443033212149, 56.99948385550241170, 0.02388180880522514787 ) ) ;
#6903 = ORIENTED_EDGE ( 'NONE', *, *, #15883, .F. ) ;
#6904 = CARTESIAN_POINT ( 'NONE',  ( -16.79901371501579632, -30.85325472854623285, -9.000000000000000000 ) ) ;
#6905 = ORIENTED_EDGE ( 'NONE', *, *, #504, .F. ) ;
#6906 = CARTESIAN_POINT ( 'NONE',  ( 54.68390685589033495, 61.69948385550240744, -6.485486291978119766 ) ) ;
#6907 = CIRCLE ( 'NONE', #1592, 5.200000000000001066 ) ;
#6908 = FACE_OUTER_BOUND ( 'NONE', #2572, .T. ) ;
#6909 = CARTESIAN_POINT ( 'NONE',  ( 55.11794222512601493, 52.19948385550240744, 3.688883143319541702 ) ) ;
#6910 = CARTESIAN_POINT ( 'NONE',  ( 20.00000000000000000, -20.00000000000000000, -23.00000000000000000 ) ) ;
#6911 = DIRECTION ( 'NONE',  ( -0.000000000000000000, -0.000000000000000000, -1.000000000000000000 ) ) ;
#6912 = VECTOR ( 'NONE', #14362, 1000.000000000000000 ) ;
#6913 = AXIS2_PLACEMENT_3D ( 'NONE', #5729, #2898, #9147 ) ;
#6914 = AXIS2_PLACEMENT_3D ( 'NONE', #13666, #6223, #18206 ) ;
#6915 = CARTESIAN_POINT ( 'NONE',  ( 52.57664461997821093, 47.40051614449765793, 8.007379884777206414 ) ) ;
#6916 = CARTESIAN_POINT ( 'NONE',  ( 50.02271294988511841, 62.49948385550240459, 6.000000000000000888 ) ) ;
#6917 = AXIS2_PLACEMENT_3D ( 'NONE', #2483, #12756, #9603 ) ;
#6918 = CYLINDRICAL_SURFACE ( 'NONE', #12860, 14.00000000000000000 ) ;
#6919 = DIRECTION ( 'NONE',  ( 1.000000000000000000, 0.000000000000000000, 0.000000000000000000 ) ) ;
#6920 = VERTEX_POINT ( 'NONE', #1431 ) ;
#6921 = EDGE_CURVE ( 'NONE', #7670, #19190, #13379, .T. ) ;
#6922 = ORIENTED_EDGE ( 'NONE', *, *, #14905, .T. ) ;
#6923 = CARTESIAN_POINT ( 'NONE',  ( -20.63749999999999929, 4.898587196589412829E-16, 4.000000000000000000 ) ) ;
#6924 =( NAMED_UNIT ( * ) SI_UNIT ( $, .STERADIAN. ) SOLID_ANGLE_UNIT ( ) );
#6925 = VERTEX_POINT ( 'NONE', #5940 ) ;
#6926 = ADVANCED_FACE ( 'NONE', ( #11902 ), #17912, .T. ) ;
#6927 = CARTESIAN_POINT ( 'NONE',  ( 54.09612160359786515, 55.69948385550240744, -5.676469297603166098 ) ) ;
#6928 = CARTESIAN_POINT ( 'NONE',  ( -54.99999999999996447, -14.99999999999998579, 15.00000000000000000 ) ) ;
#6929 = CIRCLE ( 'NONE', #4746, 1.535500000000000087 ) ;
#6930 = VERTEX_POINT ( 'NONE', #5640 ) ;
#6931 = VECTOR ( 'NONE', #13623, 1000.000000000000000 ) ;
#6932 = ORIENTED_EDGE ( 'NONE', *, *, #2872, .T. ) ;
#6933 = CARTESIAN_POINT ( 'NONE',  ( -8.134732861516020819, -1.729090847147989773, 9.000000000000000000 ) ) ;
#6934 = PRESENTATION_LAYER_ASSIGNMENT (  '', '', ( #1940 ) ) ;
#6935 = ORIENTED_EDGE ( 'NONE', *, *, #9621, .T. ) ;
#6936 = DIRECTION ( 'NONE',  ( 0.000000000000000000, 0.000000000000000000, -1.000000000000000000 ) ) ;
#6937 = VERTEX_POINT ( 'NONE', #17626 ) ;
#6938 = CARTESIAN_POINT ( 'NONE',  ( 50.02271294988512551, 54.49948385550240459, 7.000000000000000888 ) ) ;
#6939 = FACE_OUTER_BOUND ( 'NONE', #2047, .T. ) ;
#6940 = CARTESIAN_POINT ( 'NONE',  ( 52.25172492374527877, 45.40051614449766504, 7.007379884777203749 ) ) ;
#6941 = CARTESIAN_POINT ( 'NONE',  ( -6.080745460913608902, 0.5192545390863924082, -1.000000000000000000 ) ) ;
#6942 = CARTESIAN_POINT ( 'NONE',  ( 4.071447262713887127, 2.020725942163686284, -3.499999999999999556 ) ) ;
#6943 = DIRECTION ( 'NONE',  ( 0.000000000000000000, 0.000000000000000000, 1.000000000000000000 ) ) ;
#6944 = PRODUCT ( 'hex flange nut gradea_iso_ISO - 4161 - M5 - N', 'hex flange nut gradea_iso_ISO - 4161 - M5 - N', '', ( #17972 ) ) ;
#6945 = AXIS2_PLACEMENT_3D ( 'NONE', #5558, #6667, #17829 ) ;
#6946 = ORIENTED_EDGE ( 'NONE', *, *, #8565, .T. ) ;
#6947 = VERTEX_POINT ( 'NONE', #4176 ) ;
#6948 = DIRECTION ( 'NONE',  ( -0.8191520442889902442, 0.000000000000000000, -0.5735764363510482688 ) ) ;
#6949 = PRESENTATION_STYLE_ASSIGNMENT (( #8411 ) ) ;
#6950 = CARTESIAN_POINT ( 'NONE',  ( 0.000000000000000000, 0.000000000000000000, 0.000000000000000000 ) ) ;
#6951 = FACE_OUTER_BOUND ( 'NONE', #14837, .T. ) ;
#6952 = CONTEXT_DEPENDENT_SHAPE_REPRESENTATION ( #21, #10229 ) ;
#6953 = VERTEX_POINT ( 'NONE', #2724 ) ;
#6954 = CARTESIAN_POINT ( 'NONE',  ( 14.17539641854901689, -5.891203581559916636, 0.000000000000000000 ) ) ;
#6955 = VERTEX_POINT ( 'NONE', #8678 ) ;
#6956 = ORIENTED_EDGE ( 'NONE', *, *, #9256, .T. ) ;
#6957 = CARTESIAN_POINT ( 'NONE',  ( -1.000000000000000000, -14.00000000000000000, 8.999999999999998224 ) ) ;
#6958 = DIRECTION ( 'NONE',  ( 1.000000000000000000, 0.000000000000000000, 0.000000000000000000 ) ) ;
#6959 = CARTESIAN_POINT ( 'NONE',  ( 55.11794222512599362, 44.80051614449766362, -3.688883143319583446 ) ) ;
#6960 = DIRECTION ( 'NONE',  ( 0.000000000000000000, 0.000000000000000000, 1.000000000000000000 ) ) ;
#6961 = DIRECTION ( 'NONE',  ( 0.000000000000000000, 0.000000000000000000, 1.000000000000000000 ) ) ;
#6962 = CARTESIAN_POINT ( 'NONE',  ( 48.02776887271745210, 51.39948385550241028, -5.992620115222778487 ) ) ;
#6963 = LINE ( 'NONE', #3936, #16615 ) ;
#6964 = CARTESIAN_POINT ( 'NONE',  ( 56.79116909180255135, 63.79948385550241596, -4.963592699179005585 ) ) ;
#6965 = CARTESIAN_POINT ( 'NONE',  ( 45.27934281921082516, 49.70051614449766220, 6.458785618021089192 ) ) ;
#6966 = VECTOR ( 'NONE', #5635, 1000.000000000000000 ) ;
#6967 = CARTESIAN_POINT ( 'NONE',  ( 1.250000000000000000, -6.429618962271402616, 0.000000000000000000 ) ) ;
#6968 = PLANE ( 'NONE',  #653 ) ;
#6969 = CARTESIAN_POINT ( 'NONE',  ( 0.000000000000000000, 0.000000000000000000, 0.000000000000000000 ) ) ;
#6970 = ORIENTED_EDGE ( 'NONE', *, *, #12883, .T. ) ;
#6971 = ORIENTED_EDGE ( 'NONE', *, *, #5737, .T. ) ;
#6972 = CARTESIAN_POINT ( 'NONE',  ( 0.9999999999999997780, -6.008326913195983998, -0.8000000000000000444 ) ) ;
#6973 = CYLINDRICAL_SURFACE ( 'NONE', #9686, 6.000000000000001776 ) ;
#6974 = CARTESIAN_POINT ( 'NONE',  ( 44.05948171654945611, 52.20051614449765509, -4.345558710429044069 ) ) ;
#6975 = CARTESIAN_POINT ( 'NONE',  ( -0.6937372685066653943, 4.453844082567723461, -3.610536846335889116 ) ) ;
#6976 = DIRECTION ( 'NONE',  ( 0.000000000000000000, 0.4999999999999991118, -0.8660254037844390407 ) ) ;
#6977 = ORIENTED_EDGE ( 'NONE', *, *, #12523, .F. ) ;
#6978 = CARTESIAN_POINT ( 'NONE',  ( 0.000000000000000000, 0.000000000000000000, -9.999999999999998224 ) ) ;
#6979 = CARTESIAN_POINT ( 'NONE',  ( 0.5449313310647804220, 4.304185902836899835, -3.316620875263383894 ) ) ;
#6980 = CARTESIAN_POINT ( 'NONE',  ( 54.13287192849676188, 50.29948385550240175, 5.649768623646098220 ) ) ;
#6981 = DIRECTION ( 'NONE',  ( 0.000000000000000000, 0.000000000000000000, -1.000000000000000000 ) ) ;
#6982 = CARTESIAN_POINT ( 'NONE',  ( 41.58830220609386430, 46.99948385550239749, 0.02388180880523263147 ) ) ;
#6983 = CARTESIAN_POINT ( 'NONE',  ( 5.000000000000003553, -20.00000000000000000, -9.999999999999994671 ) ) ;
#6984 = ADVANCED_FACE ( 'NONE', ( #14648 ), #1234, .T. ) ;
#6985 = CARTESIAN_POINT ( 'NONE',  ( 44.03140696652198471, 45.80051614449764230, 4.306917132069485454 ) ) ;
#6986 = CARTESIAN_POINT ( 'NONE',  ( 62.49999999999998579, 45.00000000000001421, 9.999999999999998224 ) ) ;
#6987 = CARTESIAN_POINT ( 'NONE',  ( 6.327640840229819652, -2.033197012992983943, 4.999999999998298250 ) ) ;
#6988 = ORIENTED_EDGE ( 'NONE', *, *, #4232, .F. ) ;
#6989 = EDGE_CURVE ( 'NONE', #8619, #4021, #3806, .T. ) ;
#6990 = ORIENTED_EDGE ( 'NONE', *, *, #3293, .F. ) ;
#6991 = CARTESIAN_POINT ( 'NONE',  ( 55.48859070151218020, 45.00000000000002132, -4.999999999999993783 ) ) ;
#6992 = ORIENTED_EDGE ( 'NONE', *, *, #7411, .F. ) ;
#6993 = EDGE_CURVE ( 'NONE', #3706, #5480, #2879, .T. ) ;
#6994 = EDGE_CURVE ( 'NONE', #12100, #7086, #17018, .T. ) ;
#6995 = CARTESIAN_POINT ( 'NONE',  ( -2.595115354961444076, -7.673029147243174641, 0.000000000000000000 ) ) ;
#6996 = VERTEX_POINT ( 'NONE', #16631 ) ;
#6997 = DIRECTION ( 'NONE',  ( -1.000000000000000000, 0.000000000000000000, 0.000000000000000000 ) ) ;
#6998 = CARTESIAN_POINT ( 'NONE',  ( 52.25172492374522903, 59.59948385550239891, -7.007379884777227730 ) ) ;
#6999 = ADVANCED_FACE ( 'NONE', ( #242 ), #9342, .F. ) ;
#7000 = VERTEX_POINT ( 'NONE', #11011 ) ;
#7001 = DIRECTION ( 'NONE',  ( -9.858538378746663627E-23, 5.031452844637890958E-23, -1.000000000000000000 ) ) ;
#7002 = EDGE_LOOP ( 'NONE', ( #10993, #16054, #5506 ) ) ;
#7003 = CARTESIAN_POINT ( 'NONE',  ( 49.97728705011486738, 59.49948385550240459, -8.000000000000001776 ) ) ;
#7004 = DIRECTION ( 'NONE',  ( -4.082155997157844188E-16, 1.000000000000000000, 0.000000000000000000 ) ) ;
#7005 = CARTESIAN_POINT ( 'NONE',  ( 46.45491332379572924, 53.29948385550240886, -4.840751629271157874 ) ) ;
#7006 = CIRCLE ( 'NONE', #10442, 5.000000000000000888 ) ;
#7007 = DIRECTION ( 'NONE',  ( -1.000000000000000000, 0.000000000000000000, -0.000000000000000000 ) ) ;
#7008 = PLANE ( 'NONE',  #5557 ) ;
#7009 = CARTESIAN_POINT ( 'NONE',  ( 56.79116909180259398, 47.20051614449766220, 4.963592699178938972 ) ) ;
#7010 = AXIS2_PLACEMENT_3D ( 'NONE', #8647, #14438, #14724 ) ;
#7011 = EDGE_CURVE ( 'NONE', #848, #19213, #16802, .T. ) ;
#7012 = CARTESIAN_POINT ( 'NONE',  ( 55.71335778527780036, 48.90051614449766504, -1.832500667257213056 ) ) ;
#7013 = EDGE_CURVE ( 'NONE', #10609, #3916, #1142, .T. ) ;
#7014 = DIRECTION ( 'NONE',  ( -1.000000000000000000, 0.000000000000000000, 0.000000000000000000 ) ) ;
#7015 = DIRECTION ( 'NONE',  ( 0.000000000000000000, 0.000000000000000000, 1.000000000000000000 ) ) ;
#7016 = ORIENTED_EDGE ( 'NONE', *, *, #3564, .T. ) ;
#7017 = VERTEX_POINT ( 'NONE', #13573 ) ;
#7018 = FACE_OUTER_BOUND ( 'NONE', #9194, .T. ) ;
#7019 = APPLICATION_PROTOCOL_DEFINITION ( 'draft international standard', 'automotive_design', 1998, #1394 ) ;
#7020 = EDGE_LOOP ( 'NONE', ( #14938, #9884, #13680, #12286 ) ) ;
#7021 = AXIS2_PLACEMENT_3D ( 'NONE', #4930, #16909, #3658 ) ;
#7022 = CARTESIAN_POINT ( 'NONE',  ( 45.90387839640214196, 60.69948385550240033, 5.676469297603166098 ) ) ;
#7023 = CARTESIAN_POINT ( 'NONE',  ( 4.175813232069146785, -2.061359961916366057, 3.570380186727398542 ) ) ;
#7024 = ORIENTED_EDGE ( 'NONE', *, *, #9763, .T. ) ;
#7025 = EDGE_LOOP ( 'NONE', ( #9165, #18891, #7715, #13289, #1417 ) ) ;
#7026 = CIRCLE ( 'NONE', #18005, 7.500000000000000888 ) ;
#7027 = FACE_OUTER_BOUND ( 'NONE', #6729, .T. ) ;
#7028 = ORIENTED_EDGE ( 'NONE', *, *, #12633, .F. ) ;
#7029 = DIRECTION ( 'NONE',  ( 1.000000000000000000, 0.000000000000000000, 0.000000000000000000 ) ) ;
#7030 = VERTEX_POINT ( 'NONE', #148 ) ;
#7031 = CARTESIAN_POINT ( 'NONE',  ( 44.03140696652192787, 49.19948385550240033, -4.306917132069425058 ) ) ;
#7032 = DIRECTION ( 'NONE',  ( 0.000000000000000000, 0.000000000000000000, -1.000000000000000000 ) ) ;
#7033 = CARTESIAN_POINT ( 'NONE',  ( 43.33558569842706021, 47.90051614449765793, 2.141517661632167169 ) ) ;
#7034 = LINE ( 'NONE', #677, #9532 ) ;
#7035 = FACE_OUTER_BOUND ( 'NONE', #12081, .T. ) ;
#7036 = EDGE_CURVE ( 'NONE', #2713, #11891, #4938, .T. ) ;
#7037 = CARTESIAN_POINT ( 'NONE',  ( 8.978549240895586059E-17, -0.3420925509381363971, 3.500000000000000444 ) ) ;
#7038 = AXIS2_PLACEMENT_3D ( 'NONE', #14089, #14486, #8305 ) ;
#7039 = EDGE_CURVE ( 'NONE', #4201, #8542, #17275, .T. ) ;
#7040 = ORIENTED_EDGE ( 'NONE', *, *, #12394, .F. ) ;
#7041 = ORIENTED_EDGE ( 'NONE', *, *, #6051, .T. ) ;
#7042 = DIRECTION ( 'NONE',  ( -0.9768494444668812671, -0.2139279384389642935, 0.000000000000000000 ) ) ;
#7043 = SURFACE_STYLE_FILL_AREA ( #5771 ) ;
#7044 = COLOUR_RGB ( '',0.8941176470588234615, 0.8941176470588234615, 0.8941176470588234615 ) ;
#7045 = DIRECTION ( 'NONE',  ( 1.000000000000000000, 0.000000000000000000, 0.000000000000000000 ) ) ;
#7046 = CARTESIAN_POINT ( 'NONE',  ( 4.200000000000001954, 2.694222958124178486E-16, 2.200000000000001066 ) ) ;
#7047 = ORIENTED_EDGE ( 'NONE', *, *, #1273, .F. ) ;
#7048 = CARTESIAN_POINT ( 'NONE',  ( 6.541334219041338827, 5.921300567812616933, -0.03049376373817709943 ) ) ;
#7049 = ORIENTED_EDGE ( 'NONE', *, *, #3582, .T. ) ;
#7050 = VERTEX_POINT ( 'NONE', #6128 ) ;
#7051 = EDGE_CURVE ( 'NONE', #17538, #2843, #16335, .T. ) ;
#7052 = DIRECTION ( 'NONE',  ( 0.000000000000000000, -1.000000000000000000, 0.000000000000000000 ) ) ;
#7053 = DIRECTION ( 'NONE',  ( -1.000000000000000000, 0.000000000000000000, 0.000000000000000000 ) ) ;
#7054 = CARTESIAN_POINT ( 'NONE',  ( 44.30067958973594955, 48.10051614449766078, -1.875703265242155693 ) ) ;
#7055 = CARTESIAN_POINT ( 'NONE',  ( 1.999999999999998224, -3.464101615137772594, -3.142992957459239012 ) ) ;
#7056 = AXIS2_PLACEMENT_3D ( 'NONE', #12258, #13633, #18067 ) ;
#7057 = ADVANCED_FACE ( 'NONE', ( #7686 ), #6323, .T. ) ;
#7058 = CARTESIAN_POINT ( 'NONE',  ( -151.2002204621512078, -14.95906757097668027, -15.00000000000000000 ) ) ;
#7059 = CARTESIAN_POINT ( 'NONE',  ( 48.02776887271745210, 53.39948385550241028, -5.992620115222778487 ) ) ;
#7060 = CARTESIAN_POINT ( 'NONE',  ( -1.000000000000000222, -4.808326913195983821, -0.8000000000000000444 ) ) ;
#7061 = CARTESIAN_POINT ( 'NONE',  ( 54.09612160359786515, 47.69948385550240744, -5.676469297603166098 ) ) ;
#7062 = CARTESIAN_POINT ( 'NONE',  ( 52.62207051974829852, 46.60051614449764656, -7.992620115222797139 ) ) ;
#7063 = CARTESIAN_POINT ( 'NONE',  ( -20.63749999999999574, 6.613092715395707467E-16, 5.400000000000000355 ) ) ;
#7064 = VECTOR ( 'NONE', #9390, 1000.000000000000000 ) ;
#7065 = DIRECTION ( 'NONE',  ( -1.000000000000000000, -0.000000000000000000, -0.000000000000000000 ) ) ;
#7066 = CARTESIAN_POINT ( 'NONE',  ( 0.000000000000000000, 0.000000000000000000, 0.000000000000000000 ) ) ;
#7067 = ORIENTED_EDGE ( 'NONE', *, *, #12208, .F. ) ;
#7068 = CARTESIAN_POINT ( 'NONE',  ( 5.384454397937118664, 0.000000000000000000, -4.484454397937119197 ) ) ;
#7069 = VECTOR ( 'NONE', #16857, 1000.000000000000000 ) ;
#7070 = CARTESIAN_POINT ( 'NONE',  ( -9.999999999999996447, 25.00000000000001776, 15.00000000000000000 ) ) ;
#7071 = CARTESIAN_POINT ( 'NONE',  ( 54.13287192849671214, 50.70051614449766220, -5.649768623646139964 ) ) ;
#7072 = CARTESIAN_POINT ( 'NONE',  ( 6.244889965166096069, -3.924082311521025712, -3.413878157001049907 ) ) ;
#7073 = AXIS2_PLACEMENT_3D ( 'NONE', #10478, #14995, #1678 ) ;
#7074 = CYLINDRICAL_SURFACE ( 'NONE', #18719, 1.000000000000000888 ) ;
#7075 = VERTEX_POINT ( 'NONE', #4851 ) ;
#7076 = CARTESIAN_POINT ( 'NONE',  ( -154.9999999999999716, -14.99999999999999645, -15.00000000000000000 ) ) ;
#7077 = FACE_OUTER_BOUND ( 'NONE', #17440, .T. ) ;
#7078 = B_SPLINE_CURVE_WITH_KNOTS ( 'NONE', 3,
 ( #8126, #2163, #16879, #782, #14102, #9588 ),
 .UNSPECIFIED., .F., .F.,
 ( 4, 2, 4 ),
 ( 4.336808689942017736E-19, 0.001488912493401929995, 0.002977824986803859555 ),
 .UNSPECIFIED. ) ;
#7079 = CARTESIAN_POINT ( 'NONE',  ( 42.63976443033212860, 48.99948385550240459, 0.02388180880522514787 ) ) ;
#7080 = CARTESIAN_POINT ( 'NONE',  ( 6.367873360227555679, -2.886751345948119774, 4.999999999999999112 ) ) ;
#7081 = CARTESIAN_POINT ( 'NONE',  ( 45.27934281921075410, 49.29948385550240886, -6.458785618021043895 ) ) ;
#7082 = DIRECTION ( 'NONE',  ( 0.000000000000000000, 0.5000000000000011102, 0.8660254037844379305 ) ) ;
#7083 = CARTESIAN_POINT ( 'NONE',  ( 50.02271294988505446, 46.50051614449765935, -7.000000000000000888 ) ) ;
#7084 = CARTESIAN_POINT ( 'NONE',  ( 6.204449577088272605, 0.9975080636026212311, 5.000000000000000000 ) ) ;
#7085 = EDGE_LOOP ( 'NONE', ( #2543, #2443, #11047, #8419, #10414 ) ) ;
#7086 = VERTEX_POINT ( 'NONE', #1916 ) ;
#7087 = DIRECTION ( 'NONE',  ( -0.000000000000000000, -0.000000000000000000, -1.000000000000000000 ) ) ;
#7088 = ORIENTED_EDGE ( 'NONE', *, *, #11119, .T. ) ;
#7089 = DIRECTION ( 'NONE',  ( -0.9781476007338065770, 0.2079116908177552348, 0.000000000000000000 ) ) ;
#7090 = VECTOR ( 'NONE', #6314, 1000.000000000000000 ) ;
#7091 = ORIENTED_EDGE ( 'NONE', *, *, #11192, .F. ) ;
#7092 = DIRECTION ( 'NONE',  ( 0.6691306063588571273, 0.7431448254773952433, 0.000000000000000000 ) ) ;
#7093 = EDGE_CURVE ( 'NONE', #11712, #11651, #8168, .T. ) ;
#7094 = EDGE_LOOP ( 'NONE', ( #4582, #1003, #13263, #10631, #13791, #7028 ) ) ;
#7095 = CARTESIAN_POINT ( 'NONE',  ( -18.89043790736545603, -22.09056926535314602, -9.000000000000000000 ) ) ;
#7096 = ORIENTED_EDGE ( 'NONE', *, *, #1486, .F. ) ;
#7097 = CARTESIAN_POINT ( 'NONE',  ( 50.02271294988513972, 56.49948385550240459, 8.000000000000001776 ) ) ;
#7098 = PRODUCT_RELATED_PRODUCT_CATEGORY ( 'part', '', ( #6944 ) ) ;
#7099 = CARTESIAN_POINT ( 'NONE',  ( -1.250000000000001110, 0.000000000000000000, -5.575000000000000178 ) ) ;
#7100 = CLOSED_SHELL ( 'NONE', ( #12631, #11831, #18693, #15165, #9269, #16229, #17676, #2633, #10725, #68, #16303, #11112, #8303, #2982, #16106, #8285, #4003, #8699, #4247, #16011, #19312, #1618, #18572, #16493, #1721, #3774, #13649, #6111, #903, #14042, #3659, #7400, #2230, #1488, #1613, #7128, #12747, #11270 ) ) ;
#7101 = PRODUCT_DEFINITION_SHAPE ( 'NONE', 'NONE',  #17058 ) ;
#7102 = CARTESIAN_POINT ( 'NONE',  ( 56.30877334542961421, 47.99948385550239038, -0.02388180880520959434 ) ) ;
#7103 = DIRECTION ( 'NONE',  ( -0.000000000000000000, -0.000000000000000000, 1.000000000000000000 ) ) ;
#7104 = CYLINDRICAL_SURFACE ( 'NONE', #11825, 9.999999999999998224 ) ;
#7105 = CARTESIAN_POINT ( 'NONE',  ( 49.97728705011495265, 45.50051614449766646, 8.000000000000001776 ) ) ;
#7106 = ADVANCED_FACE ( 'NONE', ( #3480 ), #16815, .F. ) ;
#7107 = CARTESIAN_POINT ( 'NONE',  ( 55.11794222512599362, 50.80051614449766362, -3.688883143319583446 ) ) ;
#7108 = ADVANCED_FACE ( 'NONE', ( #15431 ), #2009, .F. ) ;
#7109 = VECTOR ( 'NONE', #11088, 1000.000000000000000 ) ;
#7110 = CARTESIAN_POINT ( 'NONE',  ( 3.972709601346593455, -3.429395227388317036, -1.191688283765307110 ) ) ;
#7111 = AXIS2_PLACEMENT_3D ( 'NONE', #10765, #13712, #13892 ) ;
#7112 = LINE ( 'NONE', #11617, #15979 ) ;
#7113 = ORIENTED_EDGE ( 'NONE', *, *, #17739, .T. ) ;
#7114 = EDGE_CURVE ( 'NONE', #40, #18188, #1718, .T. ) ;
#7115 = EDGE_CURVE ( 'NONE', #828, #2369, #19168, .T. ) ;
#7116 = EDGE_LOOP ( 'NONE', ( #2642, #18730, #4086, #8468 ) ) ;
#7117 = CARTESIAN_POINT ( 'NONE',  ( -1.000000000000000000, -14.00000000000000000, 8.999999999999998224 ) ) ;
#7118 = ORIENTED_EDGE ( 'NONE', *, *, #1011, .T. ) ;
#7119 = CARTESIAN_POINT ( 'NONE',  ( 42.63976443033212860, 60.99948385550238328, 0.02388180880522514787 ) ) ;
#7120 = B_SPLINE_CURVE_WITH_KNOTS ( 'NONE', 3,
 ( #2522, #12979, #13179, #19089, #834, #4166 ),
 .UNSPECIFIED., .F., .F.,
 ( 4, 2, 4 ),
 ( 0.01799235506992015107, 0.01945319861728521740, 0.02091404216465028373 ),
 .UNSPECIFIED. ) ;
#7121 = LINE ( 'NONE', #3898, #10900 ) ;
#7122 = CIRCLE ( 'NONE', #13067, 2.000000000000001776 ) ;
#7123 = ORIENTED_EDGE ( 'NONE', *, *, #2450, .F. ) ;
#7124 = ORIENTED_EDGE ( 'NONE', *, *, #16523, .F. ) ;
#7125 = CARTESIAN_POINT ( 'NONE',  ( 7.336184427528458230, 9.926022037524705097E-16, 8.105212085995399107 ) ) ;
#7126 = ADVANCED_FACE ( 'NONE', ( #724 ), #18680, .F. ) ;
#7127 = LINE ( 'NONE', #14104, #16932 ) ;
#7128 = ADVANCED_FACE ( 'NONE', ( #3959 ), #14236, .F. ) ;
#7129 = VERTEX_POINT ( 'NONE', #6986 ) ;
#7130 = FACE_OUTER_BOUND ( 'NONE', #13979, .T. ) ;
#7131 = ORIENTED_EDGE ( 'NONE', *, *, #5452, .F. ) ;
#7132 = AXIS2_PLACEMENT_3D ( 'NONE', #13280, #5534, #14848 ) ;
#7133 = CARTESIAN_POINT ( 'NONE',  ( 2.449293598294706513E-15, -20.00000000000000000, -9.000000000000000000 ) ) ;
#7134 = CARTESIAN_POINT ( 'NONE',  ( 50.02271294988512551, 48.49948385550240459, 7.000000000000000888 ) ) ;
#7135 = DIRECTION ( 'NONE',  ( 0.7969485188038759604, 0.6040472319084893016, -1.134471691914156900E-16 ) ) ;
#7136 = CARTESIAN_POINT ( 'NONE',  ( 57.36023556966787851, 51.00051614449763804, 0.02388180880515038476 ) ) ;
#7137 = DIRECTION ( 'NONE',  ( 0.000000000000000000, -0.000000000000000000, 1.000000000000000000 ) ) ;
#7138 = ADVANCED_FACE ( 'NONE', ( #18974 ), #8258, .F. ) ;
#7139 = PRESENTATION_STYLE_ASSIGNMENT (( #7330 ) ) ;
#7140 = FACE_OUTER_BOUND ( 'NONE', #11044, .T. ) ;
#7141 = AXIS2_PLACEMENT_3D ( 'NONE', #3660, #2196, #17101 ) ;
#7142 = AXIS2_PLACEMENT_3D ( 'NONE', #13333, #13629, #19352 ) ;
#7143 = VERTEX_POINT ( 'NONE', #17107 ) ;
#7144 = VERTEX_POINT ( 'NONE', #12966 ) ;
#7145 = CARTESIAN_POINT ( 'NONE',  ( 3.175194142252359519, -39.74634503291702003, 0.000000000000000000 ) ) ;
#7146 = LINE ( 'NONE', #9880, #10864 ) ;
#7147 = DIRECTION ( 'NONE',  ( -0.000000000000000000, -0.000000000000000000, 1.000000000000000000 ) ) ;
#7148 = MECHANICAL_DESIGN_GEOMETRIC_PRESENTATION_REPRESENTATION (  '', ( #15925 ), #3401 ) ;
#7149 = ORIENTED_EDGE ( 'NONE', *, *, #8644, .F. ) ;
#7150 = DIRECTION ( 'NONE',  ( 0.000000000000000000, 0.000000000000000000, -1.000000000000000000 ) ) ;
#7151 = VERTEX_POINT ( 'NONE', #11101 ) ;
#7152 = EDGE_LOOP ( 'NONE', ( #5751, #18300, #14175, #4456 ) ) ;
#7153 = AXIS2_PLACEMENT_3D ( 'NONE', #14687, #7438, #1564 ) ;
#7154 = CIRCLE ( 'NONE', #12162, 20.00000000000000000 ) ;
#7155 = DIRECTION ( 'NONE',  ( 1.000000000000000000, 0.000000000000000000, 0.000000000000000000 ) ) ;
#7156 = DIRECTION ( 'NONE',  ( -1.000000000000000000, 0.000000000000000000, 0.000000000000000000 ) ) ;
#7157 = CARTESIAN_POINT ( 'NONE',  ( 48.07319477248762496, 48.40051614449766504, -6.007379884777208190 ) ) ;
#7158 = FACE_BOUND ( 'NONE', #14791, .T. ) ;
#7159 = CARTESIAN_POINT ( 'NONE',  ( -14.86289650954790886, -6.617387872822862782, -9.000000000000000000 ) ) ;
#7160 = CARTESIAN_POINT ( 'NONE',  ( 53.54508667620428497, 54.29948385550241596, 4.840751629271157874 ) ) ;
#7161 = CARTESIAN_POINT ( 'NONE',  ( -5.686050877451574337, -5.768780236673276995, -1.000000000000000000 ) ) ;
#7162 = CARTESIAN_POINT ( 'NONE',  ( 45.90387839640214196, 46.69948385550240744, 5.676469297603166098 ) ) ;
#7163 = CARTESIAN_POINT ( 'NONE',  ( 43.20883090819742023, 48.20051614449766930, -4.963592699178938972 ) ) ;
#7164 = CARTESIAN_POINT ( 'NONE',  ( -154.9999999999999716, -14.99999999999999645, 15.00000000000000000 ) ) ;
#7165 = CARTESIAN_POINT ( 'NONE',  ( 0.9996874511566150590, -39.97499999999999432, 9.000000000000000000 ) ) ;
#7166 = EDGE_CURVE ( 'NONE', #8318, #2130, #3666, .T. ) ;
#7167 = TOROIDAL_SURFACE ( 'NONE', #1221, 7.900000000000002132, 0.5999999999999979794 ) ;
#7168 = APPLICATION_PROTOCOL_DEFINITION ( 'draft international standard', 'automotive_design', 1998, #14660 ) ;
#7169 = ORIENTED_EDGE ( 'NONE', *, *, #8107, .T. ) ;
#7170 = CARTESIAN_POINT ( 'NONE',  ( -154.9999999999999716, -14.99999999999999645, 4.000000000000000000 ) ) ;
#7171 = EDGE_CURVE ( 'NONE', #12831, #13489, #9628, .T. ) ;
#7172 = CARTESIAN_POINT ( 'NONE',  ( 20.00000000000000000, -20.00000000000000000, -12.00000000000000000 ) ) ;
#7173 = CARTESIAN_POINT ( 'NONE',  ( 19.30627432446641123, -14.77814480204120784, 9.000000000000000000 ) ) ;
#7174 = DIRECTION ( 'NONE',  ( 0.000000000000000000, -0.8660254037844391517, -0.4999999999999991673 ) ) ;
#7175 = ORIENTED_EDGE ( 'NONE', *, *, #3222, .T. ) ;
#7176 = AXIS2_PLACEMENT_3D ( 'NONE', #19212, #1726, #4944 ) ;
#7177 = DIRECTION ( 'NONE',  ( -0.000000000000000000, 0.000000000000000000, 1.000000000000000000 ) ) ;
#7178 = AXIS2_PLACEMENT_3D ( 'NONE', #8467, #15729, #17112 ) ;
#7179 = DIRECTION ( 'NONE',  ( -1.000000000000000000, -1.040834085586084257E-16, 0.000000000000000000 ) ) ;
#7180 = CARTESIAN_POINT ( 'NONE',  ( 42.63976443033212860, 54.99948385550241170, 0.02388180880522514787 ) ) ;
#7181 = FACE_OUTER_BOUND ( 'NONE', #17594, .T. ) ;
#7182 = CARTESIAN_POINT ( 'NONE',  ( 56.79116909180255135, 47.79948385550240886, -4.963592699179005585 ) ) ;
#7183 = DIRECTION ( 'NONE',  ( -1.000000000000000000, 0.000000000000000000, 0.000000000000000000 ) ) ;
#7184 = CARTESIAN_POINT ( 'NONE',  ( 49.97728705011495265, 47.50051614449766646, 7.000000000000000888 ) ) ;
#7185 = AXIS2_PLACEMENT_3D ( 'NONE', #17039, #8092, #12509 ) ;
#7186 = DIRECTION ( 'NONE',  ( 1.000000000000000000, 0.000000000000000000, 0.000000000000000000 ) ) ;
#7187 = VERTEX_POINT ( 'NONE', #11487 ) ;
#7188 = VERTEX_POINT ( 'NONE', #17305 ) ;
#7189 = PLANE ( 'NONE',  #9671 ) ;
#7190 = ORIENTED_EDGE ( 'NONE', *, *, #3761, .F. ) ;
#7191 = AXIS2_PLACEMENT_3D ( 'NONE', #18762, #15606, #9905 ) ;
#7192 = LINE ( 'NONE', #13267, #6541 ) ;
#7193 = VERTEX_POINT ( 'NONE', #11392 ) ;
#7194 = DIRECTION ( 'NONE',  ( 0.000000000000000000, 0.000000000000000000, 1.000000000000000000 ) ) ;
#7195 = ORIENTED_EDGE ( 'NONE', *, *, #17675, .F. ) ;
#7196 = AXIS2_PLACEMENT_3D ( 'NONE', #3005, #13192, #10432 ) ;
#7197 = LINE ( 'NONE', #2712, #11787 ) ;
#7198 = ORIENTED_EDGE ( 'NONE', *, *, #17743, .T. ) ;
#7199 = CARTESIAN_POINT ( 'NONE',  ( 49.97728705011486738, 57.49948385550241170, -8.000000000000001776 ) ) ;
#7200 = DIRECTION ( 'NONE',  ( 0.000000000000000000, 0.000000000000000000, -1.000000000000000000 ) ) ;
#7201 = CARTESIAN_POINT ( 'NONE',  ( 51.97223112728254790, 52.39948385550241028, 5.992620115222778487 ) ) ;
#7202 = CARTESIAN_POINT ( 'NONE',  ( 2.000000000000000000, 1.880445160090761061E-16, -1.535500000000000087 ) ) ;
#7203 = CARTESIAN_POINT ( 'NONE',  ( 62.49999999999998579, 20.00000000000001421, -15.00000000000000000 ) ) ;
#7204 = CARTESIAN_POINT ( 'NONE',  ( 50.02271294988505446, 48.50051614449765935, -8.000000000000001776 ) ) ;
#7205 = AXIS2_PLACEMENT_3D ( 'NONE', #10783, #16785, #9313 ) ;
#7206 = CARTESIAN_POINT ( 'NONE',  ( 55.71335778527780036, 50.90051614449765793, -1.832500667257213056 ) ) ;
#7208 = CIRCLE ( 'NONE', #18191, 4.000000000000031086 ) ;
#7207 = CARTESIAN_POINT ( 'NONE',  ( -5.130877905917148318, -39.33065161639853358, -9.000000000000000000 ) ) ;
#7209 = AXIS2_PLACEMENT_3D ( 'NONE', #8691, #14663, #2442 ) ;
#7210 = DIRECTION ( 'NONE',  ( -1.000000000000000000, 0.000000000000000000, -0.000000000000000000 ) ) ;
#7211 = EDGE_CURVE ( 'NONE', #9761, #7384, #9415, .T. ) ;
#7212 = ORIENTED_EDGE ( 'NONE', *, *, #13223, .F. ) ;
#7213 = AXIS2_PLACEMENT_3D ( 'NONE', #13647, #1796, #14017 ) ;
#7214 = ORIENTED_EDGE ( 'NONE', *, *, #17441, .T. ) ;
#7215 = CARTESIAN_POINT ( 'NONE',  ( 0.000000000000000000, 3.031088913245533423, -1.750000000000004885 ) ) ;
#7216 = VERTEX_POINT ( 'NONE', #821 ) ;
#7217 = CARTESIAN_POINT ( 'NONE',  ( 0.1739375980333736638, 5.301268757141562205, -0.8179331680533008520 ) ) ;
#7218 = DIRECTION ( 'NONE',  ( 0.8090169943749464521, 0.5877852522924744694, 0.000000000000000000 ) ) ;
#7219 = ORIENTED_EDGE ( 'NONE', *, *, #2388, .T. ) ;
#7220 = EDGE_LOOP ( 'NONE', ( #18713, #3528, #18449, #12607, #8310, #11150, #9153, #1346 ) ) ;
#7221 = CARTESIAN_POINT ( 'NONE',  ( 0.000000000000000000, 0.000000000000000000, -5.000000000000000000 ) ) ;
#7222 = VECTOR ( 'NONE', #4606, 1000.000000000000114 ) ;
#7223 = CARTESIAN_POINT ( 'NONE',  ( 5.599999999999999645, -4.041451884327386779, 0.000000000000000000 ) ) ;
#7224 = ORIENTED_EDGE ( 'NONE', *, *, #19127, .F. ) ;
#7225 = AXIS2_PLACEMENT_3D ( 'NONE', #18707, #9845, #5252 ) ;
#7226 = CARTESIAN_POINT ( 'NONE',  ( -3.114822491369819039E-15, 4.452621892014636096, 2.287832656137190668 ) ) ;
#7227 = AXIS2_PLACEMENT_3D ( 'NONE', #8759, #16325, #16618 ) ;
#7228 = EDGE_LOOP ( 'NONE', ( #11490, #10627, #9960, #15326, #749 ) ) ;
#7229 = CARTESIAN_POINT ( 'NONE',  ( -1.360585162435467455, 4.061296242128285883, -3.505054077164959203 ) ) ;
#7230 = CARTESIAN_POINT ( 'NONE',  ( 42.63976443033212860, 52.99948385550240459, 0.02388180880522514787 ) ) ;
#7231 = DIRECTION ( 'NONE',  ( -0.000000000000000000, -0.000000000000000000, -1.000000000000000000 ) ) ;
#7232 = EDGE_CURVE ( 'NONE', #17315, #8654, #13814, .T. ) ;
#7233 = CARTESIAN_POINT ( 'NONE',  ( 47.70284917648459100, 47.60051614449763946, 6.992620115222796251 ) ) ;
#7234 = CARTESIAN_POINT ( 'NONE',  ( -155.0818120241833640, -18.99916326157099533, 15.79999999999999893 ) ) ;
#7235 = CARTESIAN_POINT ( 'NONE',  ( -30.00000000000000000, -39.99999999999998579, -10.00000000000000000 ) ) ;
#7236 = CIRCLE ( 'NONE', #18218, 4.999999999999999112 ) ;
#7237 = EDGE_CURVE ( 'NONE', #7750, #4148, #13188, .T. ) ;
#7238 = EDGE_CURVE ( 'NONE', #15661, #4513, #2103, .T. ) ;
#7239 = ADVANCED_FACE ( 'NONE', ( #12778 ), #919, .F. ) ;
#7240 = ORIENTED_EDGE ( 'NONE', *, *, #5076, .F. ) ;
#7241 = ORIENTED_EDGE ( 'NONE', *, *, #17571, .T. ) ;
#7242 = CARTESIAN_POINT ( 'NONE',  ( 0.000000000000000000, 0.000000000000000000, -20.00000000000000000 ) ) ;
#7243 =( NAMED_UNIT ( * ) SI_UNIT ( $, .STERADIAN. ) SOLID_ANGLE_UNIT ( ) );
#7244 = AXIS2_PLACEMENT_3D ( 'NONE', #8773, #14751, #10526 ) ;
#7245 = ADVANCED_FACE ( 'NONE', ( #5514 ), #9822, .F. ) ;
#7246 = DIRECTION ( 'NONE',  ( -3.469446951953614682E-16, 1.000000000000000000, 0.000000000000000000 ) ) ;
#7247 = DIRECTION ( 'NONE',  ( -1.000000000000000000, 0.000000000000000000, 0.000000000000000000 ) ) ;
#7248 = ORIENTED_EDGE ( 'NONE', *, *, #2696, .F. ) ;
#7249 = CARTESIAN_POINT ( 'NONE',  ( -19.99999999999999645, -20.00000000000000000, 9.000000000000000000 ) ) ;
#7250 = EDGE_CURVE ( 'NONE', #14564, #9785, #15823, .T. ) ;
#7251 = VERTEX_POINT ( 'NONE', #8065 ) ;
#7252 = ORIENTED_EDGE ( 'NONE', *, *, #19102, .F. ) ;
#7253 =( REPRESENTATION_RELATIONSHIP ('NONE','NONE', #16703, #6546 ) REPRESENTATION_RELATIONSHIP_WITH_TRANSFORMATION ( #7845 )SHAPE_REPRESENTATION_RELATIONSHIP( ) );
#7254 = DIRECTION ( 'NONE',  ( 0.000000000000000000, 0.000000000000000000, 1.000000000000000000 ) ) ;
#7255 = DIRECTION ( 'NONE',  ( 0.000000000000000000, -1.000000000000000000, 0.000000000000000000 ) ) ;
#7256 = AXIS2_PLACEMENT_3D ( 'NONE', #11267, #17472, #17576 ) ;
#7257 = CARTESIAN_POINT ( 'NONE',  ( 53.50833635130544508, 47.30051614449766362, 4.867452303228181343 ) ) ;
#7258 = DIRECTION ( 'NONE',  ( 0.000000000000000000, -0.5000000000000012212, -0.8660254037844380415 ) ) ;
#7259 = SURFACE_STYLE_USAGE ( .BOTH. , #14798 ) ;
#7260 = CIRCLE ( 'NONE', #59, 6.000000000000001776 ) ;
#7261 = CARTESIAN_POINT ( 'NONE',  ( 51.97223112728254790, 52.39948385550241028, 5.992620115222778487 ) ) ;
#7262 = CARTESIAN_POINT ( 'NONE',  ( 2.000000000000000000, 1.773042676681340524, -2.059984127722458425E-15 ) ) ;
#7263 = CARTESIAN_POINT ( 'NONE',  ( 44.05948171654949874, 54.79948385550241596, 4.345558710429105354 ) ) ;
#7264 = ADVANCED_FACE ( 'NONE', ( #14039 ), #623, .F. ) ;
#7265 = CARTESIAN_POINT ( 'NONE',  ( 50.02271294988505446, 48.50051614449765935, -8.000000000000001776 ) ) ;
#7266 = CARTESIAN_POINT ( 'NONE',  ( 3.734041964264196878, -16.98388816369253362, -9.999999999999994671 ) ) ;
#7267 = ADVANCED_FACE ( 'NONE', ( #16487 ), #6183, .T. ) ;
#7268 = CARTESIAN_POINT ( 'NONE',  ( 0.000000000000000000, 0.000000000000000000, 0.000000000000000000 ) ) ;
#7269 = SHAPE_DEFINITION_REPRESENTATION ( #8507, #13919 ) ;
#7270 = ORIENTED_EDGE ( 'NONE', *, *, #880, .F. ) ;
#7271 = CARTESIAN_POINT ( 'NONE',  ( -2.742827927723112236, -3.035229711105190464, -3.433252694550595230 ) ) ;
#7272 = FACE_OUTER_BOUND ( 'NONE', #1323, .T. ) ;
#7273 = CARTESIAN_POINT ( 'NONE',  ( -1.747541505913277282, 3.837784562140256650, -3.503702292528906526 ) ) ;
#7274 = CARTESIAN_POINT ( 'NONE',  ( 15.51323935927256237, -7.377028694403341191, 9.000000000000000000 ) ) ;
#7275 = DIRECTION ( 'NONE',  ( 1.000000000000000000, 0.000000000000000000, 0.000000000000000000 ) ) ;
#7276 = DIRECTION ( 'NONE',  ( 1.000000000000000000, 0.000000000000000000, 0.000000000000000000 ) ) ;
#7277 = DIRECTION ( 'NONE',  ( 1.000000000000000000, 0.000000000000000000, 0.000000000000000000 ) ) ;
#7278 = CARTESIAN_POINT ( 'NONE',  ( 45.90387839640214196, 54.69948385550240744, 5.676469297603166098 ) ) ;
#7279 = DIRECTION ( 'NONE',  ( 1.000000000000000000, -1.734723475976807341E-16, 0.000000000000000000 ) ) ;
#7280 = CARTESIAN_POINT ( 'NONE',  ( 52.62207051974839089, 54.39948385550241028, 7.992620115222770494 ) ) ;
#7281 = DIRECTION ( 'NONE',  ( 1.000000000000000000, 0.000000000000000000, 0.000000000000000000 ) ) ;
#7282 = EDGE_CURVE ( 'NONE', #2267, #18424, #8970, .T. ) ;
#7283 = CARTESIAN_POINT ( 'NONE',  ( 44.03140696652198471, 49.80051614449766362, 4.306917132069485454 ) ) ;
#7284 = EDGE_CURVE ( 'NONE', #14560, #5728, #19351, .T. ) ;
#7285 = APPLICATION_CONTEXT ( 'automotive_design' ) ;
#7286 = CARTESIAN_POINT ( 'NONE',  ( 62.49999999999998579, 45.00000000000001421, 5.000000000000000000 ) ) ;
#7287 = ORIENTED_EDGE ( 'NONE', *, *, #15036, .F. ) ;
#7288 = EDGE_CURVE ( 'NONE', #468, #19337, #13045, .T. ) ;
#7289 = ORIENTED_EDGE ( 'NONE', *, *, #1257, .F. ) ;
#7290 = DIRECTION ( 'NONE',  ( 0.000000000000000000, 0.000000000000000000, 1.000000000000000000 ) ) ;
#7291 = ORIENTED_EDGE ( 'NONE', *, *, #15404, .T. ) ;
#7292 = DIRECTION ( 'NONE',  ( 0.000000000000000000, 0.000000000000000000, 1.000000000000000000 ) ) ;
#7293 = EDGE_LOOP ( 'NONE', ( #6153, #9734, #7954, #14781 ) ) ;
#7294 = DIRECTION ( 'NONE',  ( 0.000000000000000000, 0.000000000000000000, -1.000000000000000000 ) ) ;
#7295 = EDGE_LOOP ( 'NONE', ( #18594, #12238, #18039, #19184 ) ) ;
#7296 = CARTESIAN_POINT ( 'NONE',  ( -1.149999999999998135, 0.000000000000000000, -4.000000000000000000 ) ) ;
#7297 = ADVANCED_FACE ( 'NONE', ( #14416 ), #15706, .T. ) ;
#7298 = ORIENTED_EDGE ( 'NONE', *, *, #15386, .T. ) ;
#7299 =( BOUNDED_SURFACE ( )  B_SPLINE_SURFACE ( 3, 2, ( 
 ( #15103, #13433, #11960 ),
 ( #10480, #3247, #5887 ),
 ( #14900, #17963, #1474 ),
 ( #19346, #1289, #9116 ),
 ( #4318, #16484, #11854 ),
 ( #14699, #13326, #4521 ) ),
 .UNSPECIFIED., .F., .F., .T. ) 
 B_SPLINE_SURFACE_WITH_KNOTS ( ( 4, 2, 4 ),
 ( 3, 3 ),
 ( 0.02032853247518126918, 0.02278863295364821906, 0.02524873343211517240 ),
 ( 0.000000000000000000, 1.000000000000000000 ),
 .UNSPECIFIED. ) 
 GEOMETRIC_REPRESENTATION_ITEM ( )  RATIONAL_B_SPLINE_SURFACE ( (
 ( 1.000000000000000000, 0.8047781615896837382, 1.000000000000000000),
 ( 1.000000000000000000, 0.8123767586289252218, 1.000000000000000000),
 ( 1.000000000000000000, 0.8190662415564388121, 1.000000000000000000),
 ( 1.000000000000000000, 0.8192361015669026303, 1.000000000000000000),
 ( 1.000000000000000000, 0.8126135807103900266, 1.000000000000000000),
 ( 1.000000000000000000, 0.8047712338318593339, 1.000000000000000000) ) ) 
 REPRESENTATION_ITEM ( '' )  SURFACE ( )  );
#7300 = CARTESIAN_POINT ( 'NONE',  ( 41.58830220609386430, 60.99948385550241170, 0.02388180880523263147 ) ) ;
#7301 = CARTESIAN_POINT ( 'NONE',  ( -59.84999999999998721, 32.50000000000001421, -10.00000000000000178 ) ) ;
#7302 = EDGE_CURVE ( 'NONE', #19213, #5450, #5336, .T. ) ;
#7303 = CARTESIAN_POINT ( 'NONE',  ( 46.45491332379572924, 57.29948385550240175, -4.840751629271157874 ) ) ;
#7304 = CARTESIAN_POINT ( 'NONE',  ( 0.1374368770859596967, -4.808326913195983821, -0.8000000000000000444 ) ) ;
#7305 = DIRECTION ( 'NONE',  ( -0.7581610723493046322, -0.6520673188974834833, 1.125475972357111981E-16 ) ) ;
#7306 = CARTESIAN_POINT ( 'NONE',  ( 58.41169779390614281, 49.00051614449765935, 0.02388180880515032231 ) ) ;
#7307 = EDGE_CURVE ( 'NONE', #7187, #9732, #14906, .T. ) ;
#7308 = CARTESIAN_POINT ( 'NONE',  ( 46.49166364869456913, 52.30051614449766362, -4.867452303228181343 ) ) ;
#7309 = DIRECTION ( 'NONE',  ( -0.9135454576426043083, 0.4067366430757925477, 0.000000000000000000 ) ) ;
#7310 = DIRECTION ( 'NONE',  ( 0.000000000000000000, 0.000000000000000000, -1.000000000000000000 ) ) ;
#7311 = VERTEX_POINT ( 'NONE', #4058 ) ;
#7312 = ORIENTED_EDGE ( 'NONE', *, *, #18047, .T. ) ;
#7313 = DIRECTION ( 'NONE',  ( -9.858538378746663627E-23, 5.031452844637890958E-23, -1.000000000000000000 ) ) ;
#7314 = EDGE_LOOP ( 'NONE', ( #12545, #2817, #13298, #19309 ) ) ;
#7315 = CYLINDRICAL_SURFACE ( 'NONE', #2046, 1.000000000000000000 ) ;
#7316 = LINE ( 'NONE', #5650, #14988 ) ;
#7317 = ORIENTED_EDGE ( 'NONE', *, *, #4436, .T. ) ;
#7318 = CARTESIAN_POINT ( 'NONE',  ( 2.449293598294706513E-15, -20.00000000000000000, 9.000000000000000000 ) ) ;
#7319 = CARTESIAN_POINT ( 'NONE',  ( 57.36023556966787851, 47.99948385550239749, -0.02388180880522424582 ) ) ;
#7320 = AXIS2_PLACEMENT_3D ( 'NONE', #9054, #10717, #15042 ) ;
#7321 = VERTEX_POINT ( 'NONE', #13 ) ;
#7322 = CARTESIAN_POINT ( 'NONE',  ( -74.99999999999997158, 40.00000000000001421, -10.00000000000000000 ) ) ;
#7323 = ORIENTED_EDGE ( 'NONE', *, *, #11157, .T. ) ;
#7324 = CIRCLE ( 'NONE', #13885, 0.9999999999999991118 ) ;
#7325 = LINE ( 'NONE', #19220, #16044 ) ;
#7326 = CARTESIAN_POINT ( 'NONE',  ( 44.05948171654949874, 56.79948385550240886, 4.345558710429105354 ) ) ;
#7327 = DIRECTION ( 'NONE',  ( 0.9998415233556813275, -0.01780247661957949992, -2.056844117275891959E-17 ) ) ;
#7328 = CARTESIAN_POINT ( 'NONE',  ( 55.94051828345053679, 47.20051614449766220, 4.345558710429044069 ) ) ;
#7329 = DIRECTION ( 'NONE',  ( -0.8090169943749430104, -0.5877852522924791323, 0.000000000000000000 ) ) ;
#7330 = SURFACE_STYLE_USAGE ( .BOTH. , #12029 ) ;
#7331 = ORIENTED_EDGE ( 'NONE', *, *, #12619, .F. ) ;
#7332 = VECTOR ( 'NONE', #17195, 1000.000000000000000 ) ;
#7333 = VERTEX_POINT ( 'NONE', #16023 ) ;
#7334 = VERTEX_POINT ( 'NONE', #2868 ) ;
#7335 = CYLINDRICAL_SURFACE ( 'NONE', #14657, 2.649999999999988365 ) ;
#7336 = AXIS2_PLACEMENT_3D ( 'NONE', #498, #3543, #5006 ) ;
#7337 = CARTESIAN_POINT ( 'NONE',  ( 43.18075615816989199, 65.19948385550240744, -4.924951120819313743 ) ) ;
#7338 = LINE ( 'NONE', #11740, #14656 ) ;
#7339 = ORIENTED_EDGE ( 'NONE', *, *, #8476, .F. ) ;
#7340 = CARTESIAN_POINT ( 'NONE',  ( -30.00000000000000000, -3.000000000000000000, -5.999999999999998224 ) ) ;
#7341 = ORIENTED_EDGE ( 'NONE', *, *, #8447, .F. ) ;
#7342 = EDGE_LOOP ( 'NONE', ( #16954, #1148, #3926, #12086, #9214 ) ) ;
#7343 = ADVANCED_FACE ( 'NONE', ( #1582 ), #11293, .F. ) ;
#7344 = FACE_OUTER_BOUND ( 'NONE', #9471, .T. ) ;
#7345 = UNCERTAINTY_MEASURE_WITH_UNIT (LENGTH_MEASURE( 1.000000000000000082E-05 ), #10583, 'distance_accuracy_value', 'NONE');
#7346 = DIRECTION ( 'NONE',  ( 9.710251638871371392E-17, 5.969973981896233748E-17, 1.000000000000000000 ) ) ;
#7347 = AXIS2_PLACEMENT_3D ( 'NONE', #13810, #6266, #9485 ) ;
#7348 = CARTESIAN_POINT ( 'NONE',  ( 44.88205777487401349, 45.80051614449766362, 3.688883143319584779 ) ) ;
#7349 = DIRECTION ( 'NONE',  ( 0.9995235871707960351, -0.03086419753086420970, 0.000000000000000000 ) ) ;
#7350 = EDGE_CURVE ( 'NONE', #8156, #14431, #11776, .T. ) ;
#7351 = FACE_OUTER_BOUND ( 'NONE', #11105, .T. ) ;
#7352 = CARTESIAN_POINT ( 'NONE',  ( 55.11794222512601493, 58.19948385550240744, 3.688883143319541702 ) ) ;
#7353 = DIRECTION ( 'NONE',  ( 0.000000000000000000, 0.000000000000000000, 1.000000000000000000 ) ) ;
#7354 = CARTESIAN_POINT ( 'NONE',  ( 54.09612160359786515, 55.69948385550240744, -5.676469297603166098 ) ) ;
#7355 = AXIS2_PLACEMENT_3D ( 'NONE', #10428, #4563, #16718 ) ;
#7356 = CARTESIAN_POINT ( 'NONE',  ( 50.02271294988505446, 54.50051614449765935, -8.000000000000001776 ) ) ;
#7357 = EDGE_CURVE ( 'NONE', #12063, #17098, #3041, .T. ) ;
#7358 = CARTESIAN_POINT ( 'NONE',  ( 4.104070371397480876, -2.023683613428371775, -3.505122836902506922 ) ) ;
#7359 = EDGE_CURVE ( 'NONE', #12330, #6630, #4358, .T. ) ;
#7360 = CARTESIAN_POINT ( 'NONE',  ( 3.974175853610027342, 3.450041667725633143, -1.156004144283977908 ) ) ;
#7361 = ORIENTED_EDGE ( 'NONE', *, *, #14676, .T. ) ;
#7362 = LINE ( 'NONE', #5793, #17788 ) ;
#7363 = ADVANCED_FACE ( 'NONE', ( #14939 ), #6773, .T. ) ;
#7364 = DIRECTION ( 'NONE',  ( 0.000000000000000000, 0.000000000000000000, -1.000000000000000000 ) ) ;
#7365 = AXIS2_PLACEMENT_3D ( 'NONE', #1083, #12649, #2472 ) ;
#7366 = VERTEX_POINT ( 'NONE', #10424 ) ;
#7367 = CARTESIAN_POINT ( 'NONE',  ( 2.649999999999988365, 15.00000000000001599, 9.000000000000000000 ) ) ;
#7368 = CARTESIAN_POINT ( 'NONE',  ( -5.130877905917283321, -0.6693483836015015065, 0.000000000000000000 ) ) ;
#7369 = AXIS2_PLACEMENT_3D ( 'NONE', #7068, #8837, #1390 ) ;
#7370 = EDGE_CURVE ( 'NONE', #3962, #18623, #6212, .T. ) ;
#7371 = DIRECTION ( 'NONE',  ( 0.000000000000000000, 0.000000000000000000, 1.000000000000000000 ) ) ;
#7372 = EDGE_CURVE ( 'NONE', #3206, #11016, #15132, .T. ) ;
#7373 = DIRECTION ( 'NONE',  ( 0.000000000000000000, 0.000000000000000000, -1.000000000000000000 ) ) ;
#7374 = CARTESIAN_POINT ( 'NONE',  ( 3.160591952521659032, -3.281206521718069258, 0.000000000000000000 ) ) ;
#7375 = CYLINDRICAL_SURFACE ( 'NONE', #771, 3.799999999999993605 ) ;
#7376 = FACE_OUTER_BOUND ( 'NONE', #10375, .T. ) ;
#7377 = CARTESIAN_POINT ( 'NONE',  ( 54.09612160359786515, 57.69948385550240744, -5.676469297603166098 ) ) ;
#7378 = DIRECTION ( 'NONE',  ( -0.6691306063588506881, -0.7431448254774009055, 0.000000000000000000 ) ) ;
#7379 = CARTESIAN_POINT ( 'NONE',  ( 47.42335538002188144, 52.59948385550240602, 8.007379884777233059 ) ) ;
#7380 = CARTESIAN_POINT ( 'NONE',  ( 4.158806965674307854, -1.986429158307096321, -3.559403772175836256 ) ) ;
#7381 = CARTESIAN_POINT ( 'NONE',  ( 52.29715082351538769, 50.60051614449766788, -6.992620115222796251 ) ) ;
#7382 = DIRECTION ( 'NONE',  ( 0.000000000000000000, 0.000000000000000000, 1.000000000000000000 ) ) ;
#7383 = CIRCLE ( 'NONE', #4263, 2.100000000000000089 ) ;
#7384 = VERTEX_POINT ( 'NONE', #4559 ) ;
#7385 = VERTEX_POINT ( 'NONE', #338 ) ;
#7386 = DIRECTION ( 'NONE',  ( 0.000000000000000000, 0.000000000000000000, 1.000000000000000000 ) ) ;
#7387 = ORIENTED_EDGE ( 'NONE', *, *, #11676, .T. ) ;
#7388 = CIRCLE ( 'NONE', #18366, 2.649999999999988365 ) ;
#7389 = DIRECTION ( 'NONE',  ( -1.387778780781445676E-16, 1.000000000000000000, 0.000000000000000000 ) ) ;
#7390 = ORIENTED_EDGE ( 'NONE', *, *, #14048, .T. ) ;
#7391 = CARTESIAN_POINT ( 'NONE',  ( -99.99999999999997158, -23.00000000000000711, 15.00000000000000000 ) ) ;
#7392 = ORIENTED_EDGE ( 'NONE', *, *, #1250, .T. ) ;
#7393 = CYLINDRICAL_SURFACE ( 'NONE', #9595, 4.000000000000003553 ) ;
#7394 = EDGE_LOOP ( 'NONE', ( #6639, #7439, #19080, #2167 ) ) ;
#7395 = DIRECTION ( 'NONE',  ( -9.858538378746663627E-23, 5.031452844637890958E-23, -1.000000000000000000 ) ) ;
#7396 = DIRECTION ( 'NONE',  ( 0.000000000000000000, 0.4999999999999989453, -0.8660254037844391517 ) ) ;
#7397 = CIRCLE ( 'NONE', #5831, 0.9999999999999980016 ) ;
#7398 = CARTESIAN_POINT ( 'NONE',  ( 43.69122665457040000, 56.99948385550241170, 0.02388180880521036456 ) ) ;
#7399 = PLANE ( 'NONE',  #10713 ) ;
#7400 = ADVANCED_FACE ( 'NONE', ( #1623 ), #11995, .F. ) ;
#7401 = LINE ( 'NONE', #8485, #7757 ) ;
#7402 = CARTESIAN_POINT ( 'NONE',  ( 42.38452918213190657, 53.90051614449765793, 2.450534656007115508 ) ) ;
#7403 = CARTESIAN_POINT ( 'NONE',  ( 53.54508667620424234, 48.70051614449766930, -4.840751629271188961 ) ) ;
#7404 = CARTESIAN_POINT ( 'NONE',  ( 0.000000000000000000, 1.773042676681340524, -2.059984127722458425E-15 ) ) ;
#7405 = CARTESIAN_POINT ( 'NONE',  ( 0.000000000000000000, 0.000000000000000000, -15.00000000000000000 ) ) ;
#7406 = ORIENTED_EDGE ( 'NONE', *, *, #12626, .T. ) ;
#7407 = ORIENTED_EDGE ( 'NONE', *, *, #18061, .T. ) ;
#7408 = LINE ( 'NONE', #19209, #19104 ) ;
#7409 = VECTOR ( 'NONE', #2902, 1000.000000000000000 ) ;
#7410 = VERTEX_POINT ( 'NONE', #2994 ) ;
#7411 = EDGE_CURVE ( 'NONE', #7030, #8472, #13753, .T. ) ;
#7412 = CARTESIAN_POINT ( 'NONE',  ( 49.97728705011488159, 63.49948385550241170, -7.000000000000000888 ) ) ;
#7413 = DIRECTION ( 'NONE',  ( 0.1045284632676494602, 0.9945218953682738450, 0.000000000000000000 ) ) ;
#7414 = ORIENTED_EDGE ( 'NONE', *, *, #2384, .T. ) ;
#7415 = CARTESIAN_POINT ( 'NONE',  ( 0.000000000000000000, 0.000000000000000000, -9.000000000000000000 ) ) ;
#7416 = PRODUCT ( 'hub', 'hub', '', ( #8926 ) ) ;
#7417 = EDGE_CURVE ( 'NONE', #11786, #17308, #18198, .T. ) ;
#7418 = LINE ( 'NONE', #7223, #9392 ) ;
#7419 = ORIENTED_EDGE ( 'NONE', *, *, #12496, .F. ) ;
#7420 = CARTESIAN_POINT ( 'NONE',  ( 2.449293598294706513E-15, -20.00000000000000000, 9.000000000000000000 ) ) ;
#7421 = ORIENTED_EDGE ( 'NONE', *, *, #8556, .T. ) ;
#7422 = CARTESIAN_POINT ( 'NONE',  ( 52.57664461997821093, 63.40051614449765083, 8.007379884777206414 ) ) ;
#7423 = CARTESIAN_POINT ( 'NONE',  ( -160.9999999999999432, -14.99999999999999645, -9.000000000000000000 ) ) ;
#7424 = VECTOR ( 'NONE', #16133, 1000.000000000000000 ) ;
#7425 = CARTESIAN_POINT ( 'NONE',  ( 56.65037692655918988, 55.89948385550240317, -2.184720259617163762 ) ) ;
#7426 = CYLINDRICAL_SURFACE ( 'NONE', #846, 12.49999999999999645 ) ;
#7427 = AXIS2_PLACEMENT_3D ( 'NONE', #8302, #967, #9962 ) ;
#7428 = CARTESIAN_POINT ( 'NONE',  ( 44.05948171654945611, 56.20051614449764799, -4.345558710429044069 ) ) ;
#7429 = CARTESIAN_POINT ( 'NONE',  ( -20.00000000000000000, -19.99999999999999289, -23.00000000000000000 ) ) ;
#7430 = CARTESIAN_POINT ( 'NONE',  ( 0.000000000000000000, 0.000000000000000000, -0.3080913168122742518 ) ) ;
#7431 = DIRECTION ( 'NONE',  ( 0.000000000000000000, 0.000000000000000000, -1.000000000000000000 ) ) ;
#7432 = ORIENTED_EDGE ( 'NONE', *, *, #7956, .T. ) ;
#7433 = ORIENTED_EDGE ( 'NONE', *, *, #6994, .T. ) ;
#7434 = ORIENTED_EDGE ( 'NONE', *, *, #12646, .F. ) ;
#7435 = CARTESIAN_POINT ( 'NONE',  ( 1.925929944387235853E-31, 15.00000000000001599, 15.00000000000000000 ) ) ;
#7436 = VECTOR ( 'NONE', #12834, 1000.000000000000000 ) ;
#7437 = CARTESIAN_POINT ( 'NONE',  ( 56.66441430157296821, 46.09948385550240602, 2.141517661632100111 ) ) ;
#7438 = DIRECTION ( 'NONE',  ( -9.858538378746663627E-23, 5.031452844637890958E-23, -1.000000000000000000 ) ) ;
#7439 = ORIENTED_EDGE ( 'NONE', *, *, #1620, .T. ) ;
#7440 =( GEOMETRIC_REPRESENTATION_CONTEXT ( 3 ) GLOBAL_UNCERTAINTY_ASSIGNED_CONTEXT ( ( #5782 ) ) GLOBAL_UNIT_ASSIGNED_CONTEXT ( ( #1835, #18126, #4689 ) ) REPRESENTATION_CONTEXT ( 'NONE', 'WORKASPACE' ) );
#7441 = CARTESIAN_POINT ( 'NONE',  ( 0.000000000000000000, 0.000000000000000000, -0.8000000000000000444 ) ) ;
#7442 = ORIENTED_EDGE ( 'NONE', *, *, #13415, .T. ) ;
#7443 = CARTESIAN_POINT ( 'NONE',  ( 52.25172492374528588, 61.40051614449765793, 7.007379884777204637 ) ) ;
#7444 = ORIENTED_EDGE ( 'NONE', *, *, #12644, .T. ) ;
#7445 = FACE_OUTER_BOUND ( 'NONE', #2663, .T. ) ;
#7446 = CARTESIAN_POINT ( 'NONE',  ( 0.2174200650117537048, -2.185595227304857335, 3.214438021527933564 ) ) ;
#7447 = VECTOR ( 'NONE', #19148, 1000.000000000000000 ) ;
#7448 = CARTESIAN_POINT ( 'NONE',  ( 44.28664221472221385, 57.90051614449765793, 1.832500667257213722 ) ) ;
#7449 = FACE_OUTER_BOUND ( 'NONE', #6876, .T. ) ;
#7450 = PRESENTATION_STYLE_ASSIGNMENT (( #7259 ) ) ;
#7451 = CARTESIAN_POINT ( 'NONE',  ( 44.91013252490152752, 58.79948385550240175, 3.727524721679198461 ) ) ;
#7452 = DIRECTION ( 'NONE',  ( 0.000000000000000000, 0.000000000000000000, -1.000000000000000000 ) ) ;
#7453 = CARTESIAN_POINT ( 'NONE',  ( 45.86712807150323812, 55.29948385550240175, -5.649768623646098220 ) ) ;
#7454 = CARTESIAN_POINT ( 'NONE',  ( 43.18075615816994173, 51.80051614449766362, 4.924951120819380357 ) ) ;
#7455 = CARTESIAN_POINT ( 'NONE',  ( 0.000000000000000000, -4.330127018922188320, 2.500000000000010214 ) ) ;
#7456 = CARTESIAN_POINT ( 'NONE',  ( 3.880206590543185730, 3.396506438958505125, -1.117078279489029935 ) ) ;
#7457 = CARTESIAN_POINT ( 'NONE',  ( 2.449293598294706513E-15, -20.00000000000000000, 9.000000000000000000 ) ) ;
#7458 = EDGE_CURVE ( 'NONE', #14591, #3708, #7776, .T. ) ;
#7459 = APPLICATION_PROTOCOL_DEFINITION ( 'draft international standard', 'automotive_design', 1998, #18441 ) ;
#7460 = EDGE_LOOP ( 'NONE', ( #11837, #1636 ) ) ;
#7461 = CARTESIAN_POINT ( 'NONE',  ( -155.0676494111543491, -18.79939778875158396, -15.00000000000000000 ) ) ;
#7462 = AXIS2_PLACEMENT_3D ( 'NONE', #17162, #9687, #5474 ) ;
#7463 = VECTOR ( 'NONE', #15974, 1000.000000000000000 ) ;
#7464 = LINE ( 'NONE', #7368, #1254 ) ;
#7465 = CARTESIAN_POINT ( 'NONE',  ( 49.97728705011488159, 61.49948385550240459, -7.000000000000000888 ) ) ;
#7466 = PRESENTATION_LAYER_ASSIGNMENT (  '', '', ( #3103 ) ) ;
#7467 = CARTESIAN_POINT ( 'NONE',  ( 6.534224484704324709, 2.950930484791589148, 5.111161529262913561 ) ) ;
#7468 = CARTESIAN_POINT ( 'NONE',  ( -154.9999999999999716, -14.99999999999999645, -15.79999999999999893 ) ) ;
#7469 = DIRECTION ( 'NONE',  ( -0.000000000000000000, -0.000000000000000000, 1.000000000000000000 ) ) ;
#7470 = CARTESIAN_POINT ( 'NONE',  ( 52.29715082351547295, 58.39948385550238896, 6.992620115222774047 ) ) ;
#7471 = EDGE_CURVE ( 'NONE', #16922, #5141, #12091, .T. ) ;
#7472 = DIRECTION ( 'NONE',  ( 0.000000000000000000, 0.000000000000000000, 1.000000000000000000 ) ) ;
#7473 = CARTESIAN_POINT ( 'NONE',  ( 54.72065718078924590, 54.29948385550241596, 6.458785618021043895 ) ) ;
#7474 = CARTESIAN_POINT ( 'NONE',  ( 3.878096787214417862, -3.381939201670079331, -1.142309474598505181 ) ) ;
#7475 = CARTESIAN_POINT ( 'NONE',  ( 55.96859303347802239, 52.80051614449764941, -4.306917132069484566 ) ) ;
#7476 = AXIS2_PLACEMENT_3D ( 'NONE', #14266, #9661, #17136 ) ;
#7477 = DIRECTION ( 'NONE',  ( -1.000000000000000000, 0.000000000000000000, 0.000000000000000000 ) ) ;
#7479 = ORIENTED_EDGE ( 'NONE', *, *, #2108, .F. ) ;
#7478 = EDGE_CURVE ( 'NONE', #14540, #3495, #16329, .T. ) ;
#7480 = EDGE_CURVE ( 'NONE', #3535, #6538, #1807, .T. ) ;
#7481 = ORIENTED_EDGE ( 'NONE', *, *, #15267, .F. ) ;
#7482 = CARTESIAN_POINT ( 'NONE',  ( 0.2499999999999966416, -8.096141056083448362, -1.000000000000000000 ) ) ;
#7483 = ORIENTED_EDGE ( 'NONE', *, *, #18402, .T. ) ;
#7484 = DIRECTION ( 'NONE',  ( -1.000000000000000000, -0.000000000000000000, -0.000000000000000000 ) ) ;
#7485 = VECTOR ( 'NONE', #927, 1000.000000000000000 ) ;
#7486 = EDGE_CURVE ( 'NONE', #2420, #11109, #13567, .T. ) ;
#7487 = AXIS2_PLACEMENT_3D ( 'NONE', #10435, #13490, #66 ) ;
#7488 = ORIENTED_EDGE ( 'NONE', *, *, #18257, .T. ) ;
#7489 = EDGE_CURVE ( 'NONE', #15388, #6930, #6168, .T. ) ;
#7490 = CARTESIAN_POINT ( 'NONE',  ( 1.000000000000002442, -20.00000000000000000, 8.999999999999998224 ) ) ;
#7491 = VERTEX_POINT ( 'NONE', #10716 ) ;
#7492 = CARTESIAN_POINT ( 'NONE',  ( -9.999999999999994671, 20.00000000000001421, 15.00000000000000000 ) ) ;
#7493 = CARTESIAN_POINT ( 'NONE',  ( 8.500000000000000000, 2.886751345948125991, 4.999999999999999112 ) ) ;
#7494 = CARTESIAN_POINT ( 'NONE',  ( 44.88205777487398507, 59.19948385550240744, -3.688883143319540814 ) ) ;
#7495 = ADVANCED_FACE ( 'NONE', ( #10616 ), #3273, .F. ) ;
#7496 = CARTESIAN_POINT ( 'NONE',  ( -19.89043790736547379, -17.90943073464699609, -9.000000000000000000 ) ) ;
#7497 = SURFACE_STYLE_FILL_AREA ( #15331 ) ;
#7498 = CARTESIAN_POINT ( 'NONE',  ( 57.61547081786810764, 50.90051614449765793, -2.450534656007114176 ) ) ;
#7499 = CARTESIAN_POINT ( 'NONE',  ( 50.02271294988506156, 58.50051614449765225, -6.000000000000000888 ) ) ;
#7500 = DIRECTION ( 'NONE',  ( 0.000000000000000000, 0.000000000000000000, 1.000000000000000000 ) ) ;
#7501 = CYLINDRICAL_SURFACE ( 'NONE', #5966, 20.00000000000000000 ) ;
#7502 = AXIS2_PLACEMENT_3D ( 'NONE', #13150, #11675, #14913 ) ;
#7503 = ORIENTED_EDGE ( 'NONE', *, *, #7011, .F. ) ;
#7504 = CIRCLE ( 'NONE', #18475, 0.9999999999999991118 ) ;
#7505 = VERTEX_POINT ( 'NONE', #15226 ) ;
#7506 = FACE_OUTER_BOUND ( 'NONE', #2012, .T. ) ;
#7507 = ORIENTED_EDGE ( 'NONE', *, *, #12863, .T. ) ;
#7508 = CARTESIAN_POINT ( 'NONE',  ( 52.29715082351547295, 64.39948385550239607, 6.992620115222774047 ) ) ;
#7509 = DIRECTION ( 'NONE',  ( -1.000000000000000000, 0.000000000000000000, 0.000000000000000000 ) ) ;
#7510 = AXIS2_PLACEMENT_3D ( 'NONE', #7164, #8830, #13144 ) ;
#7511 = VERTEX_POINT ( 'NONE', #8864 ) ;
#7512 = DIRECTION ( 'NONE',  ( 1.000000000000000000, 0.000000000000000000, 0.000000000000000000 ) ) ;
#7513 = PLANE ( 'NONE',  #5005 ) ;
#7514 = EDGE_LOOP ( 'NONE', ( #1239, #3441, #10246, #18615 ) ) ;
#7515 = CARTESIAN_POINT ( 'NONE',  ( -160.9999999999999432, -14.99999999999999645, -6.499999999999999112 ) ) ;
#7516 = ORIENTED_EDGE ( 'NONE', *, *, #11542, .F. ) ;
#7517 = CARTESIAN_POINT ( 'NONE',  ( 54.72065718078924590, 48.29948385550240175, 6.458785618021043895 ) ) ;
#7518 = VECTOR ( 'NONE', #3167, 1000.000000000000000 ) ;
#7519 = DIRECTION ( 'NONE',  ( 0.000000000000000000, 0.000000000000000000, -1.000000000000000000 ) ) ;
#7520 = CARTESIAN_POINT ( 'NONE',  ( 44.03140696652192787, 59.19948385550238612, -4.306917132069425058 ) ) ;
#7521 = CARTESIAN_POINT ( 'NONE',  ( 2.000000000000000000, 1.773042676681340524, -2.059984127722458425E-15 ) ) ;
#7522 = DIRECTION ( 'NONE',  ( 0.000000000000000000, 0.000000000000000000, -1.000000000000000000 ) ) ;
#7523 = CARTESIAN_POINT ( 'NONE',  ( 47.70284917648459100, 51.60051614449765367, 6.992620115222796251 ) ) ;
#7524 = DIRECTION ( 'NONE',  ( 0.000000000000000000, 0.000000000000000000, -1.000000000000000000 ) ) ;
#7525 = EDGE_CURVE ( 'NONE', #7216, #15143, #14842, .T. ) ;
#7526 = DIRECTION ( 'NONE',  ( -0.000000000000000000, -0.000000000000000000, 1.000000000000000000 ) ) ;
#7527 = ORIENTED_EDGE ( 'NONE', *, *, #5306, .T. ) ;
#7528 = EDGE_CURVE ( 'NONE', #3206, #17826, #11892, .T. ) ;
#7529 = VERTEX_POINT ( 'NONE', #14028 ) ;
#7530 = VERTEX_POINT ( 'NONE', #18582 ) ;
#7531 = CARTESIAN_POINT ( 'NONE',  ( 0.4465819873849485311, -2.886751345948517677, -5.000000000000000000 ) ) ;
#7532 = CIRCLE ( 'NONE', #17888, 6.000000000000001776 ) ;
#7533 = CARTESIAN_POINT ( 'NONE',  ( 56.81924384183011512, 64.19948385550240744, 4.924951120819313743 ) ) ;
#7534 = VECTOR ( 'NONE', #2356, 1000.000000000000000 ) ;
#7535 = CIRCLE ( 'NONE', #17558, 20.00000000000000000 ) ;
#7536 = ORIENTED_EDGE ( 'NONE', *, *, #16858, .F. ) ;
#7537 = DIRECTION ( 'NONE',  ( -0.000000000000000000, -0.000000000000000000, -1.000000000000000000 ) ) ;
#7538 = ORIENTED_EDGE ( 'NONE', *, *, #7211, .T. ) ;
#7539 = CARTESIAN_POINT ( 'NONE',  ( 49.97728705011495265, 61.50051614449765935, 7.000000000000000888 ) ) ;
#7540 = EDGE_LOOP ( 'NONE', ( #13888, #14787, #4257, #1669 ) ) ;
#7541 = CYLINDRICAL_SURFACE ( 'NONE', #13496, 2.500000000000000444 ) ;
#7542 = UNCERTAINTY_MEASURE_WITH_UNIT (LENGTH_MEASURE( 1.000000000000000082E-05 ), #16270, 'distance_accuracy_value', 'NONE');
#7543 = CARTESIAN_POINT ( 'NONE',  ( -3.309651814758565180, -5.455921364805393026, -1.000000000000000000 ) ) ;
#7545 = CIRCLE ( 'NONE', #9410, 4.000000000000021316 ) ;
#7544 = CARTESIAN_POINT ( 'NONE',  ( 53.54508667620424234, 54.70051614449765509, -4.840751629271188961 ) ) ;
#7546 = DIRECTION ( 'NONE',  ( 0.000000000000000000, 0.000000000000000000, 1.000000000000000000 ) ) ;
#7547 = ADVANCED_FACE ( 'NONE', ( #2297 ), #6487, .T. ) ;
#7548 = DIRECTION ( 'NONE',  ( 0.000000000000000000, 0.000000000000000000, 1.000000000000000000 ) ) ;
#7549 = CARTESIAN_POINT ( 'NONE',  ( 50.02271294988511841, 56.49948385550240459, 6.000000000000000888 ) ) ;
#7550 = DIRECTION ( 'NONE',  ( -0.000000000000000000, -0.000000000000000000, 1.000000000000000000 ) ) ;
#7551 = CIRCLE ( 'NONE', #10981, 12.49999999999999645 ) ;
#7552 = AXIS2_PLACEMENT_3D ( 'NONE', #436, #10812, #13943 ) ;
#7553 = CARTESIAN_POINT ( 'NONE',  ( 41.58830220609386430, 52.00051614449766646, -0.02388180880514929535 ) ) ;
#7554 = DIRECTION ( 'NONE',  ( -0.000000000000000000, 0.000000000000000000, 1.000000000000000000 ) ) ;
#7555 = DIRECTION ( 'NONE',  ( -1.000000000000000000, -0.000000000000000000, -0.000000000000000000 ) ) ;
#7556 = ADVANCED_BREP_SHAPE_REPRESENTATION ( '', ( #2357, #10359 ), #1541 ) ;
#7557 = ORIENTED_EDGE ( 'NONE', *, *, #3307, .F. ) ;
#7558 = DIRECTION ( 'NONE',  ( -9.858538378746663627E-23, 5.031452844637890958E-23, -1.000000000000000000 ) ) ;
#7559 = APPLICATION_PROTOCOL_DEFINITION ( 'draft international standard', 'automotive_design', 1998, #11764 ) ;
#7560 = EDGE_LOOP ( 'NONE', ( #2059, #6529, #11689, #4455 ) ) ;
#7561 = CARTESIAN_POINT ( 'NONE',  ( 5.000000000000003553, -20.00000000000000000, 15.00000000000000355 ) ) ;
#7562 = LINE ( 'NONE', #10876, #5018 ) ;
#7563 = VECTOR ( 'NONE', #13041, 1000.000000000000000 ) ;
#7564 = CARTESIAN_POINT ( 'NONE',  ( -129.9999999999999716, -14.99999999999999645, 3.999999999999999112 ) ) ;
#7565 = CARTESIAN_POINT ( 'NONE',  ( -1.149999999999998135, 0.000000000000000000, 0.000000000000000000 ) ) ;
#7566 = CARTESIAN_POINT ( 'NONE',  ( -149.0000000000000000, -14.99999999999999645, 6.499999999999999112 ) ) ;
#7567 = CARTESIAN_POINT ( 'NONE',  ( -0.02511973781850462134, 4.877415612947412882, -3.751298745799839462 ) ) ;
#7568 = CARTESIAN_POINT ( 'NONE',  ( 52.29715082351547295, 60.39948385550239607, 6.992620115222774047 ) ) ;
#7569 = FACE_OUTER_BOUND ( 'NONE', #16394, .T. ) ;
#7570 = CARTESIAN_POINT ( 'NONE',  ( 42.39856655714566358, 50.89948385550240317, 2.493737253992119207 ) ) ;
#7571 = PLANE ( 'NONE',  #17911 ) ;
#7572 = CARTESIAN_POINT ( 'NONE',  ( 44.03140696652198471, 53.80051614449766362, 4.306917132069485454 ) ) ;
#7573 = FACE_OUTER_BOUND ( 'NONE', #14480, .T. ) ;
#7574 = VERTEX_POINT ( 'NONE', #12374 ) ;
#7575 = AXIS2_PLACEMENT_3D ( 'NONE', #6759, #16255, #10068 ) ;
#7576 =( LENGTH_UNIT ( ) NAMED_UNIT ( * ) SI_UNIT ( .MILLI., .METRE. ) );
#7577 = ORIENTED_EDGE ( 'NONE', *, *, #9501, .T. ) ;
#7578 = CARTESIAN_POINT ( 'NONE',  ( -57.64999999999994884, -14.99999999999998579, 15.00000000000000178 ) ) ;
#7579 = VERTEX_POINT ( 'NONE', #12467 ) ;
#7580 = CARTESIAN_POINT ( 'NONE',  ( -17.32050807568872841, -30.00000000000008171, -9.000000000000000000 ) ) ;
#7581 = CARTESIAN_POINT ( 'NONE',  ( 44.03140696652192787, 63.19948385550240744, -4.306917132069425058 ) ) ;
#7582 = AXIS2_PLACEMENT_3D ( 'NONE', #17517, #4078, #10044 ) ;
#7583 = CARTESIAN_POINT ( 'NONE',  ( 3.734041964264196878, -16.98388816369253362, -8.999999999999996447 ) ) ;
#7584 = ORIENTED_EDGE ( 'NONE', *, *, #4477, .T. ) ;
#7585 = DIRECTION ( 'NONE',  ( 0.000000000000000000, 0.000000000000000000, -1.000000000000000000 ) ) ;
#7586 = CARTESIAN_POINT ( 'NONE',  ( -3.098410542199071749, -7.060458129626440815, -1.000000000000000000 ) ) ;
#7587 = EDGE_CURVE ( 'NONE', #12063, #12327, #15516, .T. ) ;
#7588 = CARTESIAN_POINT ( 'NONE',  ( 51.97223112728254790, 56.39948385550241028, 5.992620115222778487 ) ) ;
#7589 = CARTESIAN_POINT ( 'NONE',  ( -20.00000000000000000, -19.99999999999999289, -20.00000000000000000 ) ) ;
#7590 =( LENGTH_UNIT ( ) NAMED_UNIT ( * ) SI_UNIT ( .MILLI., .METRE. ) );
#7591 = CARTESIAN_POINT ( 'NONE',  ( 57.60143344285435774, 51.10051614449766078, 2.493737253992045044 ) ) ;
#7592 = CARTESIAN_POINT ( 'NONE',  ( 55.11794222512599362, 52.80051614449766362, -3.688883143319583446 ) ) ;
#7593 = ADVANCED_FACE ( 'NONE', ( #3656 ), #12669, .T. ) ;
#7594 = CARTESIAN_POINT ( 'NONE',  ( 1.249999999999997558, 0.000000000000000000, 0.000000000000000000 ) ) ;
#7595 = CARTESIAN_POINT ( 'NONE',  ( -99.99999999999997158, -22.99999999999999289, 10.00000000000000000 ) ) ;
#7596 = ORIENTED_EDGE ( 'NONE', *, *, #15767, .T. ) ;
#7597 = EDGE_CURVE ( 'NONE', #13007, #2523, #18689, .T. ) ;
#7598 = EDGE_CURVE ( 'NONE', #8294, #16254, #8336, .T. ) ;
#7599 = ORIENTED_EDGE ( 'NONE', *, *, #17561, .F. ) ;
#7600 = CARTESIAN_POINT ( 'NONE',  ( 6.323268674613562013, -2.010012106699304191, -5.000000000001305622 ) ) ;
#7601 = ORIENTED_EDGE ( 'NONE', *, *, #13930, .F. ) ;
#7602 = EDGE_CURVE ( 'NONE', #3326, #9351, #5120, .T. ) ;
#7603 = CARTESIAN_POINT ( 'NONE',  ( 44.03140696652192787, 65.19948385550240744, -4.306917132069425058 ) ) ;
#7604 = CARTESIAN_POINT ( 'NONE',  ( -11.75570504584948139, -3.819660112501066518, 9.000000000000000000 ) ) ;
#7605 = VERTEX_POINT ( 'NONE', #3645 ) ;
#7606 = ORIENTED_EDGE ( 'NONE', *, *, #7764, .F. ) ;
#7607 = LINE ( 'NONE', #16249, #13156 ) ;
#7608 = CARTESIAN_POINT ( 'NONE',  ( 4.071447262713888016, 4.041451884327382338, 0.000000000000000000 ) ) ;
#7609 = ORIENTED_EDGE ( 'NONE', *, *, #14897, .T. ) ;
#7610 = CARTESIAN_POINT ( 'NONE',  ( -154.9999999999999716, -14.99999999999999645, 15.79999999999999893 ) ) ;
#7611 = ORIENTED_EDGE ( 'NONE', *, *, #12720, .F. ) ;
#7612 = CARTESIAN_POINT ( 'NONE',  ( 56.81924384183011512, 46.19948385550240744, 4.924951120819313743 ) ) ;
#7613 = DIRECTION ( 'NONE',  ( 1.000000000000000000, 0.000000000000000000, 0.000000000000000000 ) ) ;
#7614 = EDGE_CURVE ( 'NONE', #4796, #2611, #15613, .T. ) ;
#7615 = CARTESIAN_POINT ( 'NONE',  ( 56.66441430157296821, 56.09948385550240602, 2.141517661632100111 ) ) ;
#7616 = CARTESIAN_POINT ( 'NONE',  ( 8.673617379884035472E-16, 4.618802153517012954, 0.000000000000000000 ) ) ;
#7617 = EDGE_CURVE ( 'NONE', #11648, #10528, #6591, .T. ) ;
#7618 = DIRECTION ( 'NONE',  ( 0.000000000000000000, 0.000000000000000000, 1.000000000000000000 ) ) ;
#7619 = CARTESIAN_POINT ( 'NONE',  ( 54.13287192849671214, 56.70051614449766220, -5.649768623646139964 ) ) ;
#7620 = CARTESIAN_POINT ( 'NONE',  ( -2.000000000000006661, 3.464101615137750834, 0.000000000000000000 ) ) ;
#7621 = LINE ( 'NONE', #18129, #2580 ) ;
#7622 = CARTESIAN_POINT ( 'NONE',  ( -4.197477534772231955, 0.8522413273724368521, -3.505042416683225692 ) ) ;
#7623 = ORIENTED_EDGE ( 'NONE', *, *, #11758, .T. ) ;
#7624 = EDGE_LOOP ( 'NONE', ( #13108, #12044 ) ) ;
#7625 = ORIENTED_EDGE ( 'NONE', *, *, #3181, .T. ) ;
#7626 = DIRECTION ( 'NONE',  ( 1.000000000000000000, -0.000000000000000000, 0.000000000000000000 ) ) ;
#7627 = CARTESIAN_POINT ( 'NONE',  ( 45.31609314410967926, 64.69948385550240744, 6.485486291978119766 ) ) ;
#7628 = CARTESIAN_POINT ( 'NONE',  ( 0.3126073911696399255, 2.020725942163686284, -3.499999999999999556 ) ) ;
#7629 = ORIENTED_EDGE ( 'NONE', *, *, #16761, .F. ) ;
#7630 = DIRECTION ( 'NONE',  ( -0.000000000000000000, -0.000000000000000000, 1.000000000000000000 ) ) ;
#7631 = ORIENTED_EDGE ( 'NONE', *, *, #18778, .F. ) ;
#7632 = CARTESIAN_POINT ( 'NONE',  ( 54.13287192849671214, 56.70051614449766220, -5.649768623646139964 ) ) ;
#7633 = ORIENTED_EDGE ( 'NONE', *, *, #11189, .F. ) ;
#7634 = CARTESIAN_POINT ( 'NONE',  ( -154.9999999999999716, -14.99999999999999645, 15.00000000000000000 ) ) ;
#7635 = CARTESIAN_POINT ( 'NONE',  ( -32.00000000000000000, -1.000000000000000000, 6.000000000000001776 ) ) ;
#7636 = EDGE_CURVE ( 'NONE', #10464, #16376, #17006, .T. ) ;
#7637 = CARTESIAN_POINT ( 'NONE',  ( 55.11794222512599362, 52.80051614449766362, -3.688883143319583446 ) ) ;
#7638 = CARTESIAN_POINT ( 'NONE',  ( -19.76107906696389094, -23.08216711247160546, 9.000000000000000000 ) ) ;
#7639 = VECTOR ( 'NONE', #13475, 1000.000000000000000 ) ;
#7640 = EDGE_CURVE ( 'NONE', #15612, #9304, #1465, .T. ) ;
#7641 = DIRECTION ( 'NONE',  ( -0.000000000000000000, -0.000000000000000000, -1.000000000000000000 ) ) ;
#7642 = CARTESIAN_POINT ( 'NONE',  ( 49.97728705011488870, 59.49948385550240459, -6.000000000000000888 ) ) ;
#7643 = LINE ( 'NONE', #6178, #1315 ) ;
#7644 = CIRCLE ( 'NONE', #13591, 20.00000000000000000 ) ;
#7645 = CARTESIAN_POINT ( 'NONE',  ( 57.61547081786810764, 52.90051614449766504, -2.450534656007114176 ) ) ;
#7646 = CARTESIAN_POINT ( 'NONE',  ( -4.000000000000000000, -1.560351142792950618, -0.2242961665059814425 ) ) ;
#7647 = CARTESIAN_POINT ( 'NONE',  ( 4.086262629614029862, 4.082406995609985323, 0.07093633357110586124 ) ) ;
#7648 = VERTEX_POINT ( 'NONE', #16908 ) ;
#7649 = PLANE ( 'NONE',  #19062 ) ;
#7650 = ITEM_DEFINED_TRANSFORMATION ( 'NONE', 'NONE', #17839,  #10359 ) ;
#7651 = ORIENTED_EDGE ( 'NONE', *, *, #16710, .T. ) ;
#7652 = CARTESIAN_POINT ( 'NONE',  ( 62.49999999999998579, 45.00000000000001421, 0.000000000000000000 ) ) ;
#7653 = EDGE_CURVE ( 'NONE', #15786, #14856, #14923, .T. ) ;
#7654 = CARTESIAN_POINT ( 'NONE',  ( 62.50000000000000000, 32.50000000000001421, 9.999999999999998224 ) ) ;
#7655 = APPLICATION_CONTEXT ( 'automotive_design' ) ;
#7656 = ADVANCED_FACE ( 'NONE', ( #6687 ), #13934, .T. ) ;
#7657 = CARTESIAN_POINT ( 'NONE',  ( 45.86712807150323812, 61.29948385550240886, -5.649768623646098220 ) ) ;
#7658 = CYLINDRICAL_SURFACE ( 'NONE', #13051, 24.99999999999999289 ) ;
#7659 = DIRECTION ( 'NONE',  ( -0.000000000000000000, -0.000000000000000000, -1.000000000000000000 ) ) ;
#7660 = DIRECTION ( 'NONE',  ( -0.9989677110047502362, -0.04542589977017699732, 6.931730960091013400E-15 ) ) ;
#7661 = CARTESIAN_POINT ( 'NONE',  ( 54.13287192849676188, 58.29948385550240175, 5.649768623646098220 ) ) ;
#7662 = LINE ( 'NONE', #13643, #10691 ) ;
#7663 = CARTESIAN_POINT ( 'NONE',  ( 56.81924384183011512, 54.19948385550241454, 4.924951120819313743 ) ) ;
#7664 = DIRECTION ( 'NONE',  ( 1.000000000000000000, 0.000000000000000000, -0.000000000000000000 ) ) ;
#7665 = CARTESIAN_POINT ( 'NONE',  ( 50.02271294988505446, 52.50051614449765935, -7.000000000000000888 ) ) ;
#7666 = CONICAL_SURFACE ( 'NONE', #4556, 2.059999999999998721, 0.9599310885968738161 ) ;
#7667 = CARTESIAN_POINT ( 'NONE',  ( -52.34999999999998010, -14.99999999999998579, 15.00000000000000000 ) ) ;
#7668 = CIRCLE ( 'NONE', #2370, 15.00000000000000000 ) ;
#7669 =( NAMED_UNIT ( * ) SI_UNIT ( $, .STERADIAN. ) SOLID_ANGLE_UNIT ( ) );
#7670 = VERTEX_POINT ( 'NONE', #11187 ) ;
#7671 = CIRCLE ( 'NONE', #11726, 4.000000000000021316 ) ;
#7672 = CARTESIAN_POINT ( 'NONE',  ( 6.534838248920897819, 2.951765777552411318, -5.112608298763837489 ) ) ;
#7673 = ORIENTED_EDGE ( 'NONE', *, *, #10566, .F. ) ;
#7674 = CARTESIAN_POINT ( 'NONE',  ( 43.34962307344078880, 48.10051614449766078, -2.184720259617096705 ) ) ;
#7675 = DIRECTION ( 'NONE',  ( 0.000000000000000000, 0.000000000000000000, 1.000000000000000000 ) ) ;
#7676 = CARTESIAN_POINT ( 'NONE',  ( 52.80949999999998568, 4.898587196589412829E-16, -4.000000000000000000 ) ) ;
#7677 = ORIENTED_EDGE ( 'NONE', *, *, #11907, .F. ) ;
#7678 = DIRECTION ( 'NONE',  ( -1.000000000000000000, 0.000000000000000000, 1.224646799147353207E-16 ) ) ;
#7679 = CYLINDRICAL_SURFACE ( 'NONE', #10136, 8.000000000000007105 ) ;
#7680 = CARTESIAN_POINT ( 'NONE',  ( 51.92680522751233951, 57.59948385550240602, -6.007379884777223289 ) ) ;
#7681 = DIRECTION ( 'NONE',  ( -1.000000000000000000, 0.000000000000000000, 0.000000000000000000 ) ) ;
#7682 = CARTESIAN_POINT ( 'NONE',  ( 73.00000000000000000, 1.000000000000000000, -5.999999999999998224 ) ) ;
#7683 = CARTESIAN_POINT ( 'NONE',  ( 56.79116909180259398, 55.20051614449766220, 4.963592699178938972 ) ) ;
#7684 = AXIS2_PLACEMENT_3D ( 'NONE', #7848, #9126, #16400 ) ;
#7685 = CARTESIAN_POINT ( 'NONE',  ( 56.30877334542961421, 55.00051614449766646, 0.02388180880515774693 ) ) ;
#7686 = FACE_OUTER_BOUND ( 'NONE', #14495, .T. ) ;
#7687 = CARTESIAN_POINT ( 'NONE',  ( 6.323279575528418128, -5.335162385627848280, -0.7592276814619393077 ) ) ;
#7688 = VERTEX_POINT ( 'NONE', #3559 ) ;
#7689 = EDGE_LOOP ( 'NONE', ( #15238, #15062, #17120, #11910 ) ) ;
#7690 = CARTESIAN_POINT ( 'NONE',  ( 6.095462721915160920, 1.047438013718291705, -5.000000000000000000 ) ) ;
#7691 = ORIENTED_EDGE ( 'NONE', *, *, #9992, .F. ) ;
#7692 = ADVANCED_FACE ( 'NONE', ( #4841 ), #10802, .T. ) ;
#7693 = CARTESIAN_POINT ( 'NONE',  ( 14.14213562373095101, -25.00000000000000711, -50.00000000000000000 ) ) ;
#7694 = ORIENTED_EDGE ( 'NONE', *, *, #14779, .T. ) ;
#7695 = CARTESIAN_POINT ( 'NONE',  ( 3.175194142251959395, -0.2536549670829221781, 9.000000000000000000 ) ) ;
#7696 = EDGE_CURVE ( 'NONE', #13512, #6867, #2092, .T. ) ;
#7697 = VECTOR ( 'NONE', #759, 1000.000000000000114 ) ;
#7698 = CARTESIAN_POINT ( 'NONE',  ( 45.86712807150323812, 51.29948385550240175, -5.649768623646098220 ) ) ;
#7699 = ORIENTED_EDGE ( 'NONE', *, *, #7640, .T. ) ;
#7700 = DIRECTION ( 'NONE',  ( -0.000000000000000000, -0.000000000000000000, 1.000000000000000000 ) ) ;
#7701 = ORIENTED_EDGE ( 'NONE', *, *, #13276, .F. ) ;
#7702 = CARTESIAN_POINT ( 'NONE',  ( 49.97728705011486738, 47.49948385550240459, -8.000000000000001776 ) ) ;
#7703 = CARTESIAN_POINT ( 'NONE',  ( -2.500000000000000888, 0.000000000000000000, -4.974599999999998801 ) ) ;
#7704 = EDGE_CURVE ( 'NONE', #3574, #2792, #16504, .T. ) ;
#7705 = CARTESIAN_POINT ( 'NONE',  ( 44.05948171654949874, 58.79948385550240886, 4.345558710429105354 ) ) ;
#7706 = LINE ( 'NONE', #13685, #18261 ) ;
#7707 = AXIS2_PLACEMENT_3D ( 'NONE', #16183, #12054, #16577 ) ;
#7708 = CARTESIAN_POINT ( 'NONE',  ( 42.63976443033212860, 56.00051614449765935, -0.02388180880514948964 ) ) ;
#7709 = ADVANCED_FACE ( 'NONE', ( #3370 ), #11408, .F. ) ;
#7710 = DIRECTION ( 'NONE',  ( -0.000000000000000000, 0.000000000000000000, 1.000000000000000000 ) ) ;
#7711 = ADVANCED_FACE ( 'NONE', ( #8911 ), #9006, .T. ) ;
#7712 = CARTESIAN_POINT ( 'NONE',  ( 11.75570504584926468, -3.819660112500910198, -9.000000000000000000 ) ) ;
#7713 = ORIENTED_EDGE ( 'NONE', *, *, #7636, .F. ) ;
#7714 = VECTOR ( 'NONE', #6031, 1000.000000000000000 ) ;
#7715 = ORIENTED_EDGE ( 'NONE', *, *, #2876, .T. ) ;
#7716 = ORIENTED_EDGE ( 'NONE', *, *, #8061, .F. ) ;
#7717 = DIRECTION ( 'NONE',  ( 0.000000000000000000, 0.000000000000000000, 1.000000000000000000 ) ) ;
#7718 = EDGE_CURVE ( 'NONE', #13101, #2111, #17391, .T. ) ;
#7719 = CARTESIAN_POINT ( 'NONE',  ( 54.09612160359786515, 45.69948385550240744, -5.676469297603166098 ) ) ;
#7720 = EDGE_CURVE ( 'NONE', #12017, #444, #14605, .T. ) ;
#7721 = DIRECTION ( 'NONE',  ( 0.03086419753086420623, 0.9995235871707959241, -0.000000000000000000 ) ) ;
#7722 = VERTEX_POINT ( 'NONE', #17754 ) ;
#7723 = FACE_OUTER_BOUND ( 'NONE', #6794, .T. ) ;
#7724 = VECTOR ( 'NONE', #10036, 1000.000000000000000 ) ;
#7725 = EDGE_LOOP ( 'NONE', ( #8874, #10715, #3987, #5167 ) ) ;
#7726 = CARTESIAN_POINT ( 'NONE',  ( 55.96859303347802239, 56.80051614449764941, -4.306917132069484566 ) ) ;
#7727 = ORIENTED_EDGE ( 'NONE', *, *, #10126, .T. ) ;
#7728 = VECTOR ( 'NONE', #15672, 1000.000000000000000 ) ;
#7729 = EDGE_CURVE ( 'NONE', #16659, #3811, #218, .T. ) ;
#7730 = DIRECTION ( 'NONE',  ( 1.000000000000000000, 0.000000000000000000, 0.000000000000000000 ) ) ;
#7731 = UNCERTAINTY_MEASURE_WITH_UNIT (LENGTH_MEASURE( 1.000000000000000082E-05 ), #13743, 'distance_accuracy_value', 'NONE');
#7732 = CARTESIAN_POINT ( 'NONE',  ( 19.89043790736549155, -22.09056926535286891, -9.000000000000000000 ) ) ;
#7733 = EDGE_CURVE ( 'NONE', #5826, #13491, #17055, .T. ) ;
#7734 = CARTESIAN_POINT ( 'NONE',  ( 43.69122665457040000, 58.00051614449765935, -0.02388180880515696977 ) ) ;
#7735 = CARTESIAN_POINT ( 'NONE',  ( -3.417495597855351487E-15, 4.207632145829744097, -2.712167343862822655 ) ) ;
#7736 = CIRCLE ( 'NONE', #1164, 5.000000000000000000 ) ;
#7737 = ADVANCED_FACE ( 'NONE', ( #18767 ), #2948, .F. ) ;
#7738 = DIRECTION ( 'NONE',  ( 0.000000000000000000, 0.000000000000000000, 1.000000000000000000 ) ) ;
#7739 = CARTESIAN_POINT ( 'NONE',  ( 44.30067958973596376, 54.89948385550240317, 1.875703265242204099 ) ) ;
#7740 = CARTESIAN_POINT ( 'NONE',  ( 62.49999999999998579, 45.00000000000001421, 0.000000000000000000 ) ) ;
#7741 = CARTESIAN_POINT ( 'NONE',  ( 54.72065718078918906, 50.70051614449766220, -6.458785618021089192 ) ) ;
#7742 = CARTESIAN_POINT ( 'NONE',  ( 6.092449800118089343, -3.827241605636891641, 3.371023086195408247 ) ) ;
#7743 = AXIS2_PLACEMENT_3D ( 'NONE', #10010, #5607, #16014 ) ;
#7744 = EDGE_LOOP ( 'NONE', ( #10973, #6946, #14302, #11154 ) ) ;
#7745 = CYLINDRICAL_SURFACE ( 'NONE', #17804, 0.7499999999999997780 ) ;
#7746 = AXIS2_PLACEMENT_3D ( 'NONE', #9386, #289, #16574 ) ;
#7747 = ORIENTED_EDGE ( 'NONE', *, *, #6221, .T. ) ;
#7748 = FILL_AREA_STYLE ('',( #9403 ) ) ;
#7749 = PRODUCT_CONTEXT ( 'NONE', #17919, 'mechanical' ) ;
#7750 = VERTEX_POINT ( 'NONE', #18871 ) ;
#7751 = LINE ( 'NONE', #1880, #13313 ) ;
#7752 = FACE_OUTER_BOUND ( 'NONE', #1222, .T. ) ;
#7753 = AXIS2_PLACEMENT_3D ( 'NONE', #18564, #5106, #11075 ) ;
#7754 = AXIS2_PLACEMENT_3D ( 'NONE', #207, #3060, #15003 ) ;
#7755 = CARTESIAN_POINT ( 'NONE',  ( 42.63976443033212149, 64.99948385550240459, 0.02388180880522514787 ) ) ;
#7756 = DIRECTION ( 'NONE',  ( -0.000000000000000000, -0.000000000000000000, -1.000000000000000000 ) ) ;
#7757 = VECTOR ( 'NONE', #1332, 1000.000000000000000 ) ;
#7758 = CARTESIAN_POINT ( 'NONE',  ( 2.449293598294706513E-15, -20.00000000000000000, -8.999999999999998224 ) ) ;
#7759 = CYLINDRICAL_SURFACE ( 'NONE', #13390, 8.099999999999999645 ) ;
#7760 = CARTESIAN_POINT ( 'NONE',  ( 42.63976443033212860, 60.99948385550238328, 0.02388180880522514787 ) ) ;
#7761 = CARTESIAN_POINT ( 'NONE',  ( -16.79901371501580698, -30.85325472854621864, 0.000000000000000000 ) ) ;
#7762 = CARTESIAN_POINT ( 'NONE',  ( 57.60143344285433642, 59.89948385550240317, -2.493737253992118319 ) ) ;
#7763 = CARTESIAN_POINT ( 'NONE',  ( 55.96859303347802239, 56.80051614449764230, -4.306917132069484566 ) ) ;
#7764 = EDGE_CURVE ( 'NONE', #16855, #15857, #1778, .T. ) ;
#7765 = DIRECTION ( 'NONE',  ( 0.000000000000000000, 0.000000000000000000, 1.000000000000000000 ) ) ;
#7766 = LINE ( 'NONE', #7667, #11909 ) ;
#7767 = EDGE_CURVE ( 'NONE', #17357, #15934, #17296, .T. ) ;
#7768 = CIRCLE ( 'NONE', #15268, 20.00000000000000000 ) ;
#7769 = VERTEX_POINT ( 'NONE', #8820 ) ;
#7770 = DIRECTION ( 'NONE',  ( 0.000000000000000000, 0.000000000000000000, -1.000000000000000000 ) ) ;
#7771 =( GEOMETRIC_REPRESENTATION_CONTEXT ( 3 ) GLOBAL_UNCERTAINTY_ASSIGNED_CONTEXT ( ( #10279 ) ) GLOBAL_UNIT_ASSIGNED_CONTEXT ( ( #17868, #4136, #7930 ) ) REPRESENTATION_CONTEXT ( 'NONE', 'WORKASPACE' ) );
#7772 = CARTESIAN_POINT ( 'NONE',  ( 52.29715082351539479, 48.60051614449766078, -6.992620115222796251 ) ) ;
#7773 = DIRECTION ( 'NONE',  ( -0.000000000000000000, -0.000000000000000000, 1.000000000000000000 ) ) ;
#7774 = CARTESIAN_POINT ( 'NONE',  ( 13.99999999999999822, 1.971681346627238735E-16, -1.610000000000000098 ) ) ;
#7775 = ORIENTED_EDGE ( 'NONE', *, *, #18888, .T. ) ;
#7776 = LINE ( 'NONE', #13474, #7090 ) ;
#7777 = VECTOR ( 'NONE', #14587, 1000.000000000000000 ) ;
#7778 = DIRECTION ( 'NONE',  ( -0.000000000000000000, -0.000000000000000000, 1.000000000000000000 ) ) ;
#7779 = CIRCLE ( 'NONE', #10263, 2.649999999999985700 ) ;
#7780 = CARTESIAN_POINT ( 'NONE',  ( 48.07319477248768180, 64.59948385550241312, 6.007379884777225953 ) ) ;
#7781 = DIRECTION ( 'NONE',  ( 0.5000000000000108802, -0.8660254037844323793, 0.000000000000000000 ) ) ;
#7782 = CARTESIAN_POINT ( 'NONE',  ( 54.72065718078918906, 60.70051614449766930, -6.458785618021089192 ) ) ;
#7783 = CARTESIAN_POINT ( 'NONE',  ( 43.69122665457040000, 54.00051614449765935, -0.02388180880515696977 ) ) ;
#7784 = DIRECTION ( 'NONE',  ( 0.000000000000000000, 0.000000000000000000, -1.000000000000000000 ) ) ;
#7785 = CARTESIAN_POINT ( 'NONE',  ( 6.362374563308273778, -3.415000007734520171, -4.302769906043296011 ) ) ;
#7786 = ORIENTED_EDGE ( 'NONE', *, *, #7943, .F. ) ;
#7787 = ORIENTED_EDGE ( 'NONE', *, *, #4827, .F. ) ;
#7788 = CARTESIAN_POINT ( 'NONE',  ( -74.99999999999997158, 40.00000000000001421, 10.00000000000000000 ) ) ;
#7789 = ORIENTED_EDGE ( 'NONE', *, *, #7039, .T. ) ;
#7790 = CIRCLE ( 'NONE', #14031, 0.7500000000000002220 ) ;
#7791 = LINE ( 'NONE', #3294, #10732 ) ;
#7792 = EDGE_LOOP ( 'NONE', ( #18822, #13695, #7287, #18409 ) ) ;
#7793 = CARTESIAN_POINT ( 'NONE',  ( 0.000000000000000000, 0.000000000000000000, 0.000000000000000000 ) ) ;
#7794 = CARTESIAN_POINT ( 'NONE',  ( 55.94051828345050836, 53.79948385550240175, -4.345558710429103577 ) ) ;
#7795 = ORIENTED_EDGE ( 'NONE', *, *, #12431, .T. ) ;
#7796 = AXIS2_PLACEMENT_3D ( 'NONE', #1002, #10002, #17285 ) ;
#7797 = CARTESIAN_POINT ( 'NONE',  ( 6.518095160331714766, -2.933089652807550074, -5.080260301817226321 ) ) ;
#7798 = ORIENTED_EDGE ( 'NONE', *, *, #1065, .T. ) ;
#7799 = CARTESIAN_POINT ( 'NONE',  ( 50.02271294988513972, 46.49948385550240459, 8.000000000000001776 ) ) ;
#7800 = CARTESIAN_POINT ( 'NONE',  ( 3.679171394226031122, 2.494631558665830973, -0.3503314178412474389 ) ) ;
#7801 = CARTESIAN_POINT ( 'NONE',  ( 45.86712807150323812, 63.29948385550240886, -5.649768623646098220 ) ) ;
#7802 = DIRECTION ( 'NONE',  ( -0.000000000000000000, -0.000000000000000000, -1.000000000000000000 ) ) ;
#7803 =( LENGTH_UNIT ( ) NAMED_UNIT ( * ) SI_UNIT ( .MILLI., .METRE. ) );
#7804 = CARTESIAN_POINT ( 'NONE',  ( 42.63976443033212860, 54.00051614449766646, -0.02388180880514948964 ) ) ;
#7805 = VECTOR ( 'NONE', #11914, 1000.000000000000114 ) ;
#7806 = EDGE_CURVE ( 'NONE', #15978, #17028, #10546, .T. ) ;
#7807 = VECTOR ( 'NONE', #18303, 1000.000000000000000 ) ;
#7808 = CARTESIAN_POINT ( 'NONE',  ( -11.75570504584937481, -36.18033988749900942, 9.000000000000000000 ) ) ;
#7809 = CARTESIAN_POINT ( 'NONE',  ( 52.25172492374522903, 51.59948385550240602, -7.007379884777225953 ) ) ;
#7810 = CARTESIAN_POINT ( 'NONE',  ( 0.000000000000000000, 0.000000000000000000, -5.000000000000000888 ) ) ;
#7811 = VECTOR ( 'NONE', #5899, 1000.000000000000000 ) ;
#7812 = ORIENTED_EDGE ( 'NONE', *, *, #306, .F. ) ;
#7813 = ORIENTED_EDGE ( 'NONE', *, *, #9310, .T. ) ;
#7814 = DIRECTION ( 'NONE',  ( -0.000000000000000000, -1.000000000000000000, -0.000000000000000000 ) ) ;
#7815 = CARTESIAN_POINT ( 'NONE',  ( 47.74827507625478518, 50.59948385550238470, 7.007379884777227730 ) ) ;
#7816 = CARTESIAN_POINT ( 'NONE',  ( -19.02113032590308705, -13.81966011250110249, -9.000000000000000000 ) ) ;
#7817 = ORIENTED_EDGE ( 'NONE', *, *, #5434, .T. ) ;
#7818 = DIRECTION ( 'NONE',  ( -1.000000000000000000, 0.000000000000000000, 0.000000000000000000 ) ) ;
#7819 = CIRCLE ( 'NONE', #316, 5.575000000000000178 ) ;
#7820 = EDGE_CURVE ( 'NONE', #16421, #18142, #10381, .T. ) ;
#7821 = ORIENTED_EDGE ( 'NONE', *, *, #7166, .T. ) ;
#7822 = CARTESIAN_POINT ( 'NONE',  ( 42.63976443033212149, 58.00051614449765225, -0.02388180880514948964 ) ) ;
#7823 = VERTEX_POINT ( 'NONE', #1468 ) ;
#7824 = DIRECTION ( 'NONE',  ( -0.000000000000000000, -0.000000000000000000, 1.000000000000000000 ) ) ;
#7825 = DIRECTION ( 'NONE',  ( 1.000000000000000000, -1.734723475976807341E-16, -0.000000000000000000 ) ) ;
#7826 = VECTOR ( 'NONE', #4939, 1000.000000000000000 ) ;
#7827 = B_SPLINE_CURVE_WITH_KNOTS ( 'NONE', 3,
 ( #17191, #17003, #11284, #14323, #3749, #9715, #5117, #9811, #15714, #2294 ),
 .UNSPECIFIED., .F., .F.,
 ( 4, 2, 2, 2, 4 ),
 ( 0.000000000000000000, 0.003112635120760290971, 0.004668952681140444913, 0.005447111461330522535, 0.006225270241520600156 ),
 .UNSPECIFIED. ) ;
#7828 = CARTESIAN_POINT ( 'NONE',  ( 55.08986747509849380, 57.20051614449766220, 3.727524721679155384 ) ) ;
#7829 = CARTESIAN_POINT ( 'NONE',  ( -74.99999999999997158, 20.00000000000001421, 15.00000000000000000 ) ) ;
#7830 = ADVANCED_FACE ( 'NONE', ( #13427 ), #11952, .F. ) ;
#7831 =( NAMED_UNIT ( * ) SI_UNIT ( $, .STERADIAN. ) SOLID_ANGLE_UNIT ( ) );
#7832 = EDGE_CURVE ( 'NONE', #3492, #18521, #16476, .T. ) ;
#7833 = CARTESIAN_POINT ( 'NONE',  ( 53.54508667620428497, 64.29948385550240175, 4.840751629271157874 ) ) ;
#7834 = CARTESIAN_POINT ( 'NONE',  ( 62.50000000000000000, 20.00000000000001421, -9.999999999999998224 ) ) ;
#7835 = CARTESIAN_POINT ( 'NONE',  ( 42.39856655714564226, 62.10051614449765367, -2.493737253992044156 ) ) ;
#7836 = EDGE_CURVE ( 'NONE', #17914, #8777, #10857, .T. ) ;
#7837 = AXIS2_PLACEMENT_3D ( 'NONE', #18634, #9298, #577 ) ;
#7838 = AXIS2_PLACEMENT_3D ( 'NONE', #1057, #16155, #3902 ) ;
#7839 = ORIENTED_EDGE ( 'NONE', *, *, #14172, .T. ) ;
#7840 = DIRECTION ( 'NONE',  ( -0.000000000000000000, -0.000000000000000000, -1.000000000000000000 ) ) ;
#7842 = ORIENTED_EDGE ( 'NONE', *, *, #11653, .F. ) ;
#7841 = EDGE_CURVE ( 'NONE', #8147, #9166, #1673, .T. ) ;
#7843 = EDGE_CURVE ( 'NONE', #18140, #16659, #6474, .T. ) ;
#7844 =( NAMED_UNIT ( * ) SI_UNIT ( $, .STERADIAN. ) SOLID_ANGLE_UNIT ( ) );
#7845 = ITEM_DEFINED_TRANSFORMATION ( 'NONE', 'NONE', #19096,  #10359 ) ;
#7846 = CIRCLE ( 'NONE', #15360, 2.649999999999985700 ) ;
#7847 = ORIENTED_EDGE ( 'NONE', *, *, #16374, .T. ) ;
#7848 = CARTESIAN_POINT ( 'NONE',  ( 19.89043790736544892, -17.90943073464672608, 9.000000000000000000 ) ) ;
#7849 = CARTESIAN_POINT ( 'NONE',  ( -0.1085714285714285687, -3.798448662927795372, 0.000000000000000000 ) ) ;
#7850 = DIRECTION ( 'NONE',  ( 0.000000000000000000, 0.000000000000000000, 1.000000000000000000 ) ) ;
#7851 = CIRCLE ( 'NONE', #15680, 2.499999999999999556 ) ;
#7852 = CARTESIAN_POINT ( 'NONE',  ( 2.449293598294706513E-15, -20.00000000000000000, -9.000000000000000000 ) ) ;
#7853 = AXIS2_PLACEMENT_3D ( 'NONE', #2086, #10894, #17002 ) ;
#7854 = VECTOR ( 'NONE', #16145, 1000.000000000000000 ) ;
#7855 = DIRECTION ( 'NONE',  ( 0.000000000000000000, -0.000000000000000000, -1.000000000000000000 ) ) ;
#7856 = ADVANCED_FACE ( 'NONE', ( #4894 ), #390, .F. ) ;
#7857 = DIRECTION ( 'NONE',  ( -1.000000000000000000, 0.000000000000000000, -0.000000000000000000 ) ) ;
#7858 = EDGE_CURVE ( 'NONE', #13420, #8876, #12424, .T. ) ;
#7859 = CARTESIAN_POINT ( 'NONE',  ( 55.08986747509847248, 47.79948385550240886, -3.727524721679197572 ) ) ;
#7860 = CARTESIAN_POINT ( 'NONE',  ( 3.951447005078451813, 1.347150628109126558, 3.500000000000000444 ) ) ;
#7861 = CARTESIAN_POINT ( 'NONE',  ( 56.81924384183011512, 62.19948385550240744, 4.924951120819313743 ) ) ;
#7862 = CARTESIAN_POINT ( 'NONE',  ( 56.65037692655921120, 55.10051614449766078, 2.184720259617097593 ) ) ;
#7863 = DIRECTION ( 'NONE',  ( 0.000000000000000000, 0.000000000000000000, 1.000000000000000000 ) ) ;
#7864 = CARTESIAN_POINT ( 'NONE',  ( -154.9999999999999716, -14.99999999999999645, -15.79999999999999893 ) ) ;
#7865 =( LENGTH_UNIT ( ) NAMED_UNIT ( * ) SI_UNIT ( .MILLI., .METRE. ) );
#7866 = VECTOR ( 'NONE', #13397, 1000.000000000000000 ) ;
#7867 = ORIENTED_EDGE ( 'NONE', *, *, #17008, .F. ) ;
#7868 = AXIS2_PLACEMENT_3D ( 'NONE', #3763, #6696, #5418 ) ;
#7869 = CARTESIAN_POINT ( 'NONE',  ( 6.533910050139693837, 2.950514251728067361, -5.110440592449059238 ) ) ;
#7870 = CARTESIAN_POINT ( 'NONE',  ( 43.33558569842706021, 45.90051614449765793, 2.141517661632167169 ) ) ;
#7871 = CARTESIAN_POINT ( 'NONE',  ( 4.082498951862918446, -2.020725942163685840, 3.500000000000002220 ) ) ;
#7872 = CARTESIAN_POINT ( 'NONE',  ( 1.250000000000000000, -6.429618962271402616, -1.000000000000000000 ) ) ;
#7873 = VERTEX_POINT ( 'NONE', #4608 ) ;
#7874 = DIRECTION ( 'NONE',  ( -0.000000000000000000, -0.000000000000000000, 1.000000000000000000 ) ) ;
#7875 = CARTESIAN_POINT ( 'NONE',  ( 2.000000000000000000, 0.000000000000000000, 0.000000000000000000 ) ) ;
#7876 = EDGE_CURVE ( 'NONE', #13768, #18910, #13616, .T. ) ;
#7877 = CARTESIAN_POINT ( 'NONE',  ( 48.02776887271745210, 61.39948385550240317, -5.992620115222778487 ) ) ;
#7878 = LINE ( 'NONE', #2097, #2773 ) ;
#7879 = EDGE_CURVE ( 'NONE', #7366, #2510, #14299, .T. ) ;
#7880 = CARTESIAN_POINT ( 'NONE',  ( 52.57664461997821093, 57.40051614449767214, 8.007379884777206414 ) ) ;
#7881 = CARTESIAN_POINT ( 'NONE',  ( 55.08986747509849380, 55.20051614449766220, 3.727524721679155384 ) ) ;
#7882 = EDGE_CURVE ( 'NONE', #17851, #12908, #12334, .T. ) ;
#7883 = CIRCLE ( 'NONE', #13519, 4.000000000000003553 ) ;
#7884 = DIRECTION ( 'NONE',  ( -1.000000000000000000, 0.000000000000000000, 0.000000000000000000 ) ) ;
#7885 = CARTESIAN_POINT ( 'NONE',  ( 6.207530437345013752, -3.810448612250145750, -3.400109403952246367 ) ) ;
#7886 = ORIENTED_EDGE ( 'NONE', *, *, #5800, .F. ) ;
#7887 = ORIENTED_EDGE ( 'NONE', *, *, #8658, .F. ) ;
#7888 = CYLINDRICAL_SURFACE ( 'NONE', #14047, 5.400000000000000355 ) ;
#7889 = ORIENTED_EDGE ( 'NONE', *, *, #2799, .T. ) ;
#7890 = PLANE ( 'NONE',  #1874 ) ;
#7891 = EDGE_LOOP ( 'NONE', ( #9935, #2214, #3323, #4886 ) ) ;
#7892 = CARTESIAN_POINT ( 'NONE',  ( 62.49999999999998579, 32.50000000000001421, 9.999999999999998224 ) ) ;
#7893 = CARTESIAN_POINT ( 'NONE',  ( 52.25172492374522903, 51.59948385550240602, -7.007379884777227730 ) ) ;
#7894 = ADVANCED_FACE ( 'NONE', ( #16864 ), #9292, .F. ) ;
#7895 = ORIENTED_EDGE ( 'NONE', *, *, #9516, .T. ) ;
#7896 = DIRECTION ( 'NONE',  ( 0.9995917534020515305, -0.02857142857142857054, 0.000000000000000000 ) ) ;
#7897 = VERTEX_POINT ( 'NONE', #7919 ) ;
#7898 = CARTESIAN_POINT ( 'NONE',  ( 52.57664461997811856, 55.59948385550240602, -8.007379884777229506 ) ) ;
#7899 = CARTESIAN_POINT ( 'NONE',  ( 0.000000000000000000, 0.000000000000000000, 3.299999999999999822 ) ) ;
#7900 = EDGE_CURVE ( 'NONE', #4021, #3495, #4916, .T. ) ;
#7901 = CARTESIAN_POINT ( 'NONE',  ( 48.02776887271745210, 47.39948385550241028, -5.992620115222778487 ) ) ;
#7902 = CARTESIAN_POINT ( 'NONE',  ( 4.055492966679600464, 2.385006769472780785, 3.005124364834443451 ) ) ;
#7903 = CARTESIAN_POINT ( 'NONE',  ( 49.97728705011495265, 63.50051614449765935, 7.000000000000000888 ) ) ;
#7904 = DIRECTION ( 'NONE',  ( -0.000000000000000000, -0.000000000000000000, 1.000000000000000000 ) ) ;
#7905 = AXIS2_PLACEMENT_3D ( 'NONE', #15136, #11803, #15230 ) ;
#7906 = CARTESIAN_POINT ( 'NONE',  ( 56.66441430157296821, 52.09948385550240602, 2.141517661632100111 ) ) ;
#7907 = DIRECTION ( 'NONE',  ( 1.000000000000000000, 0.000000000000000000, 0.000000000000000000 ) ) ;
#7908 = VERTEX_POINT ( 'NONE', #15281 ) ;
#7909 = CARTESIAN_POINT ( 'NONE',  ( 1.925929944387235853E-31, 15.00000000000001599, 9.000000000000000000 ) ) ;
#7910 = CARTESIAN_POINT ( 'NONE',  ( 44.05948171654949874, 50.79948385550238754, 4.345558710429105354 ) ) ;
#7911 = CARTESIAN_POINT ( 'NONE',  ( 20.00000000000000000, -20.00000000000000000, -12.00000000000000000 ) ) ;
#7912 = ORIENTED_EDGE ( 'NONE', *, *, #7480, .F. ) ;
#7913 = FACE_OUTER_BOUND ( 'NONE', #6094, .T. ) ;
#7914 = ORIENTED_EDGE ( 'NONE', *, *, #13840, .T. ) ;
#7915 = CARTESIAN_POINT ( 'NONE',  ( 52.29715082351539479, 62.60051614449766078, -6.992620115222796251 ) ) ;
#7916 = ORIENTED_EDGE ( 'NONE', *, *, #5306, .F. ) ;
#7917 = FACE_OUTER_BOUND ( 'NONE', #8369, .T. ) ;
#7918 = UNCERTAINTY_MEASURE_WITH_UNIT (LENGTH_MEASURE( 1.000000000000000082E-05 ), #10001, 'distance_accuracy_value', 'NONE');
#7919 = CARTESIAN_POINT ( 'NONE',  ( 12.54977455159103705, -4.427487078051979275, -9.000000000000000000 ) ) ;
#7920 = CARTESIAN_POINT ( 'NONE',  ( -154.9999999999999716, -14.99999999999999645, -15.00000000000000000 ) ) ;
#7921 =( BOUNDED_SURFACE ( )  B_SPLINE_SURFACE ( 3, 2, ( 
 ( #2360, #8221, #6747 ),
 ( #12731, #18732, #5281 ),
 ( #11252, #17264, #3824 ),
 ( #9786, #8312, #14291 ),
 ( #18839, #17358, #6844 ),
 ( #12833, #5383, #11354 ) ),
 .UNSPECIFIED., .F., .F., .T. ) 
 B_SPLINE_SURFACE_WITH_KNOTS ( ( 4, 2, 4 ),
 ( 3, 3 ),
 ( 0.02027065861071770947, 0.02273072267836921331, 0.02519078674602071716 ),
 ( 0.000000000000000000, 1.000000000000000000 ),
 .UNSPECIFIED. ) 
 GEOMETRIC_REPRESENTATION_ITEM ( )  RATIONAL_B_SPLINE_SURFACE ( (
 ( 1.000000000000000000, 0.8047781708337304885, 1.000000000000000000),
 ( 1.000000000000000000, 0.8123765190705307671, 1.000000000000000000),
 ( 1.000000000000000000, 0.8190656277163975707, 1.000000000000000000),
 ( 1.000000000000000000, 0.8192366903512159348, 1.000000000000000000),
 ( 1.000000000000000000, 0.8126138454302893610, 1.000000000000000000),
 ( 1.000000000000000000, 0.8047712246031417660, 1.000000000000000000) ) ) 
 REPRESENTATION_ITEM ( '' )  SURFACE ( )  );
#7922 = CARTESIAN_POINT ( 'NONE',  ( 53.50833635130544508, 63.30051614449767072, 4.867452303228181343 ) ) ;
#7923 = CARTESIAN_POINT ( 'NONE',  ( 0.2499999999999966416, -8.096141056083448362, -1.000000000000000000 ) ) ;
#7924 = PRESENTATION_STYLE_ASSIGNMENT (( #13716 ) ) ;
#7925 = DIRECTION ( 'NONE',  ( -1.000000000000000000, 0.000000000000000000, 0.000000000000000000 ) ) ;
#7926 = CARTESIAN_POINT ( 'NONE',  ( 54.68390685589039890, 59.30051614449766362, 6.485486291978072693 ) ) ;
#7927 = ORIENTED_EDGE ( 'NONE', *, *, #11062, .F. ) ;
#7928 = VERTEX_POINT ( 'NONE', #4708 ) ;
#7929 = DIRECTION ( 'NONE',  ( 1.040834085586084257E-16, -1.000000000000000000, 0.000000000000000000 ) ) ;
#7930 =( NAMED_UNIT ( * ) SI_UNIT ( $, .STERADIAN. ) SOLID_ANGLE_UNIT ( ) );
#7931 = ORIENTED_EDGE ( 'NONE', *, *, #2816, .F. ) ;
#7932 = DIRECTION ( 'NONE',  ( -1.000000000000000000, 0.000000000000000000, 0.000000000000000000 ) ) ;
#7933 = VERTEX_POINT ( 'NONE', #7635 ) ;
#7934 = CARTESIAN_POINT ( 'NONE',  ( 4.000000000000000000, -2.309401076758514915, -5.000000000000000000 ) ) ;
#7935 = EDGE_CURVE ( 'NONE', #4800, #18559, #15184, .T. ) ;
#7936 = CARTESIAN_POINT ( 'NONE',  ( 4.175813232069146785, 2.061359961916365613, -3.570380186727397653 ) ) ;
#7937 = EDGE_CURVE ( 'NONE', #11089, #15436, #12118, .T. ) ;
#7938 = DIRECTION ( 'NONE',  ( -1.000000000000000000, -0.000000000000000000, -0.000000000000000000 ) ) ;
#7939 = UNCERTAINTY_MEASURE_WITH_UNIT (LENGTH_MEASURE( 1.000000000000000082E-05 ), #13431, 'distance_accuracy_value', 'NONE');
#7940 = DIRECTION ( 'NONE',  ( 1.000000000000000000, -0.000000000000000000, -0.000000000000000000 ) ) ;
#7941 = AXIS2_PLACEMENT_3D ( 'NONE', #8746, #17301, #1109 ) ;
#7942 = CARTESIAN_POINT ( 'NONE',  ( 19.97007065299863271, -21.09374499507102740, 0.000000000000000000 ) ) ;
#7943 = EDGE_CURVE ( 'NONE', #10379, #12513, #5860, .T. ) ;
#7944 = EDGE_CURVE ( 'NONE', #2791, #1433, #13059, .T. ) ;
#7945 = LINE ( 'NONE', #14113, #17784 ) ;
#7946 = CARTESIAN_POINT ( 'NONE',  ( 54.13287192849676188, 62.29948385550240886, 5.649768623646098220 ) ) ;
#7947 = PLANE ( 'NONE',  #18548 ) ;
#7948 = CARTESIAN_POINT ( 'NONE',  ( 42.39856655714566358, 62.89948385550240317, 2.493737253992119207 ) ) ;
#7949 = CARTESIAN_POINT ( 'NONE',  ( 44.05948171654945611, 60.20051614449764799, -4.345558710429044069 ) ) ;
#7950 = ADVANCED_FACE ( 'NONE', ( #6447 ), #12428, .T. ) ;
#7951 = CYLINDRICAL_SURFACE ( 'NONE', #2764, 4.800000000000000711 ) ;
#7952 = DIRECTION ( 'NONE',  ( -0.7071067811865530128, 0.000000000000000000, 0.7071067811865421326 ) ) ;
#7953 = VECTOR ( 'NONE', #15911, 1000.000000000000000 ) ;
#7954 = ORIENTED_EDGE ( 'NONE', *, *, #12189, .T. ) ;
#7955 = EDGE_CURVE ( 'NONE', #8262, #7251, #3240, .T. ) ;
#7956 = EDGE_CURVE ( 'NONE', #2523, #17668, #5538, .T. ) ;
#7957 = FACE_OUTER_BOUND ( 'NONE', #17157, .T. ) ;
#7958 = CARTESIAN_POINT ( 'NONE',  ( 45.90387839640208512, 48.30051614449765651, -5.676469297603124353 ) ) ;
#7959 = CARTESIAN_POINT ( 'NONE',  ( 43.33558569842703179, 63.09948385550240602, -2.141517661632099223 ) ) ;
#7960 = CARTESIAN_POINT ( 'NONE',  ( -14.14213562373094568, -25.00000000000000000, -20.00000000000000000 ) ) ;
#7961 = VERTEX_POINT ( 'NONE', #15097 ) ;
#7962 = DIRECTION ( 'NONE',  ( -0.000000000000000000, -0.000000000000000000, -1.000000000000000000 ) ) ;
#7963 = DIRECTION ( 'NONE',  ( -1.000000000000000000, 0.000000000000000000, 0.000000000000000000 ) ) ;
#7964 = CARTESIAN_POINT ( 'NONE',  ( 51.92680522751233951, 61.59948385550240602, -6.007379884777223289 ) ) ;
#7965 = CARTESIAN_POINT ( 'NONE',  ( -2.000000000000000000, -6.429618962271402616, -1.000000000000000000 ) ) ;
#7966 = CARTESIAN_POINT ( 'NONE',  ( 44.05948171654949874, 46.79948385550238754, 4.345558710429105354 ) ) ;
#7967 = CARTESIAN_POINT ( 'NONE',  ( -3.355112389629170799, 2.681727112203152963, -0.2256878752776689534 ) ) ;
#7968 = CARTESIAN_POINT ( 'NONE',  ( 43.18075615816994173, 61.80051614449766362, 4.924951120819380357 ) ) ;
#7969 = AXIS2_PLACEMENT_3D ( 'NONE', #12827, #14384, #19023 ) ;
#7970 = CARTESIAN_POINT ( 'NONE',  ( 55.96859303347802239, 44.80051614449767072, -4.306917132069484566 ) ) ;
#7971 = CARTESIAN_POINT ( 'NONE',  ( -4.158233816355195955, -0.4370479853238878887, -9.000000000000000000 ) ) ;
#7972 = CARTESIAN_POINT ( 'NONE',  ( 10.00000000000000000, 25.00000000000001776, -15.00000000000000000 ) ) ;
#7973 = VECTOR ( 'NONE', #5798, 1000.000000000000000 ) ;
#7974 = ORIENTED_EDGE ( 'NONE', *, *, #1677, .T. ) ;
#7975 = ORIENTED_EDGE ( 'NONE', *, *, #16957, .F. ) ;
#7976 = CARTESIAN_POINT ( 'NONE',  ( 54.65205120807737416, 44.75923773080658918, -4.999999999999772626 ) ) ;
#7977 = ORIENTED_EDGE ( 'NONE', *, *, #7767, .T. ) ;
#7978 = CARTESIAN_POINT ( 'NONE',  ( -2.649999999999988365, 15.00000000000001599, 15.00000000000000000 ) ) ;
#7979 = AXIS2_PLACEMENT_3D ( 'NONE', #17171, #2668, #11556 ) ;
#7980 = VERTEX_POINT ( 'NONE', #8401 ) ;
#7981 = DIRECTION ( 'NONE',  ( 0.02857142857142857054, -0.9995917534020515305, 0.000000000000000000 ) ) ;
#7982 = CARTESIAN_POINT ( 'NONE',  ( 55.96859303347805081, 54.19948385550240033, 4.306917132069425058 ) ) ;
#7983 = ORIENTED_EDGE ( 'NONE', *, *, #2384, .F. ) ;
#7984 = CARTESIAN_POINT ( 'NONE',  ( 62.49999999999998579, 45.00000000000001421, -5.000000000000000000 ) ) ;
#7985 = ORIENTED_EDGE ( 'NONE', *, *, #19121, .T. ) ;
#7986 = CARTESIAN_POINT ( 'NONE',  ( 57.60143344285433642, 53.89948385550240317, -2.493737253992118319 ) ) ;
#7987 = LINE ( 'NONE', #13960, #14514 ) ;
#7988 = VECTOR ( 'NONE', #15112, 1000.000000000000000 ) ;
#7989 = CARTESIAN_POINT ( 'NONE',  ( 50.02271294988512551, 62.49948385550240459, 7.000000000000000888 ) ) ;
#7990 = CARTESIAN_POINT ( 'NONE',  ( 2.449293598294706513E-15, -20.00000000000000000, 9.000000000000000000 ) ) ;
#7991 = CARTESIAN_POINT ( 'NONE',  ( -9.999999999999998224, 15.00000000000001776, 15.00000000000000000 ) ) ;
#7992 = CARTESIAN_POINT ( 'NONE',  ( 54.09612160359792199, 59.30051614449766362, 5.676469297603124353 ) ) ;
#7993 = DIRECTION ( 'NONE',  ( 1.000000000000000000, 0.000000000000000000, 0.000000000000000000 ) ) ;
#7994 = CARTESIAN_POINT ( 'NONE',  ( 42.63976443033212860, 60.99948385550238328, 0.02388180880522514787 ) ) ;
#7995 = LINE ( 'NONE', #6526, #9712 ) ;
#7996 = EDGE_LOOP ( 'NONE', ( #4401, #3006, #18894, #4684 ) ) ;
#7997 = EDGE_CURVE ( 'NONE', #18339, #13933, #3710, .T. ) ;
#7998 = ORIENTED_EDGE ( 'NONE', *, *, #10276, .T. ) ;
#7999 = CARTESIAN_POINT ( 'NONE',  ( 18.68843350152500093, -27.12337372732038432, 9.000000000000000000 ) ) ;
#8000 = SHAPE_REPRESENTATION_RELATIONSHIP ( 'NONE' , 'NONE' ,  #4039, #14807 ) ;
#8001 = AXIS2_PLACEMENT_3D ( 'NONE', #15663, #1852, #668 ) ;
#8002 = EDGE_CURVE ( 'NONE', #4766, #14054, #6469, .T. ) ;
#8003 = CARTESIAN_POINT ( 'NONE',  ( 43.33558569842703179, 49.09948385550240602, -2.141517661632099223 ) ) ;
#8004 = DIRECTION ( 'NONE',  ( 0.000000000000000000, 0.000000000000000000, -1.000000000000000000 ) ) ;
#8005 = ORIENTED_EDGE ( 'NONE', *, *, #7767, .F. ) ;
#8006 = ORIENTED_EDGE ( 'NONE', *, *, #17208, .T. ) ;
#8007 = CARTESIAN_POINT ( 'NONE',  ( -3.799999999999999378, 4.653657836759941744E-16, -0.8000000000000000444 ) ) ;
#8008 = AXIS2_PLACEMENT_3D ( 'NONE', #19025, #3715, #11539 ) ;
#8009 = ORIENTED_EDGE ( 'NONE', *, *, #5246, .F. ) ;
#8010 = CARTESIAN_POINT ( 'NONE',  ( -150.9999999999999432, -14.99999999999999645, 17.00000000000000000 ) ) ;
#8011 = EDGE_LOOP ( 'NONE', ( #138, #4385, #2726, #17426 ) ) ;
#8012 = DIRECTION ( 'NONE',  ( 0.000000000000000000, 1.000000000000000000, 0.000000000000000000 ) ) ;
#8013 = B_SPLINE_CURVE_WITH_KNOTS ( 'NONE', 3,
 ( #15046, #3374, #1627, #3100, #13375, #13758 ),
 .UNSPECIFIED., .F., .F.,
 ( 4, 2, 4 ),
 ( 0.01506847346324404271, 0.01653041426658209689, 0.01799235506992015107 ),
 .UNSPECIFIED. ) ;
#8014 = CARTESIAN_POINT ( 'NONE',  ( -154.9999999999999716, -14.99999999999999645, 15.79999999999999893 ) ) ;
#8015 = CARTESIAN_POINT ( 'NONE',  ( 49.97728705011494554, 63.50051614449765935, 6.000000000000000888 ) ) ;
#8016 = DIRECTION ( 'NONE',  ( 0.9997908153927442809, -0.02045300604585054832, 2.695122805014890206E-17 ) ) ;
#8017 = DIRECTION ( 'NONE',  ( 1.000000000000000000, 0.000000000000000000, 0.000000000000000000 ) ) ;
#8018 = CARTESIAN_POINT ( 'NONE',  ( 41.58830220609386430, 60.00051614449765935, -0.02388180880514929535 ) ) ;
#8019 = ORIENTED_EDGE ( 'NONE', *, *, #10638, .T. ) ;
#8020 = EDGE_LOOP ( 'NONE', ( #684, #16341 ) ) ;
#8021 = PLANE ( 'NONE',  #11835 ) ;
#8022 = CARTESIAN_POINT ( 'NONE',  ( -3.160591952521660364, -3.281206521718067037, -0.8000000000000000444 ) ) ;
#8023 = ITEM_DEFINED_TRANSFORMATION ( 'NONE', 'NONE', #5289,  #10359 ) ;
#8024 = ORIENTED_EDGE ( 'NONE', *, *, #11061, .T. ) ;
#8025 = VECTOR ( 'NONE', #13848, 1000.000000000000000 ) ;
#8026 = DIRECTION ( 'NONE',  ( 0.000000000000000000, 0.000000000000000000, 1.000000000000000000 ) ) ;
#8027 = CARTESIAN_POINT ( 'NONE',  ( 17.32050807568866091, -9.999999999999797495, -9.000000000000000000 ) ) ;
#8028 = EDGE_LOOP ( 'NONE', ( #386, #19403, #9426, #16669, #7812 ) ) ;
#8029 =( BOUNDED_SURFACE ( )  B_SPLINE_SURFACE ( 3, 2, ( 
 ( #837, #12495, #546 ),
 ( #11216, #5055, #18411 ),
 ( #18698, #6810, #14253 ),
 ( #1936, #9550, #3498 ),
 ( #12798, #10927, #17032 ),
 ( #8083, #16835, #6424 ) ),
 .UNSPECIFIED., .F., .F., .F. ) 
 B_SPLINE_SURFACE_WITH_KNOTS ( ( 4, 2, 4 ),
 ( 3, 3 ),
 ( 0.01652267773200353021, 0.01858309280828997212, 0.02064350788457641403 ),
 ( 0.000000000000000000, 1.000000000000000000 ),
 .UNSPECIFIED. ) 
 GEOMETRIC_REPRESENTATION_ITEM ( )  RATIONAL_B_SPLINE_SURFACE ( (
 ( 1.000000000000000000, 0.8047780975688292315, 1.000000000000000000),
 ( 1.000000000000000000, 0.8123789546324570177, 1.000000000000000000),
 ( 1.000000000000000000, 0.8190677982988761041, 1.000000000000000000),
 ( 1.000000000000000000, 0.8192346069552172150, 1.000000000000000000),
 ( 1.000000000000000000, 0.8126126759768884655, 1.000000000000000000),
 ( 1.000000000000000000, 0.8047712639311999094, 1.000000000000000000) ) ) 
 REPRESENTATION_ITEM ( '' )  SURFACE ( )  );
#8030 = CARTESIAN_POINT ( 'NONE',  ( -4.999999999999998224, -20.00000000000000000, 9.000000000000000000 ) ) ;
#8031 = DIRECTION ( 'NONE',  ( 0.000000000000000000, 0.000000000000000000, 1.000000000000000000 ) ) ;
#8032 = CARTESIAN_POINT ( 'NONE',  ( 2.449293598294706513E-15, -20.00000000000000000, -9.000000000000000000 ) ) ;
#8033 = CIRCLE ( 'NONE', #15237, 2.000000000000000000 ) ;
#8034 = CARTESIAN_POINT ( 'NONE',  ( 10.00000000000000000, 25.00000000000001776, 15.00000000000000000 ) ) ;
#8035 = CARTESIAN_POINT ( 'NONE',  ( 47.70284917648453415, 65.39948385550239607, -6.992620115222774047 ) ) ;
#8036 = CYLINDRICAL_SURFACE ( 'NONE', #3155, 20.00000000000000000 ) ;
#8037 = AXIS2_PLACEMENT_3D ( 'NONE', #8014, #6836, #11243 ) ;
#8038 = CARTESIAN_POINT ( 'NONE',  ( 43.18075615816989199, 59.19948385550240744, -4.924951120819313743 ) ) ;
#8039 = EDGE_CURVE ( 'NONE', #9546, #17411, #14616, .T. ) ;
#8040 = CARTESIAN_POINT ( 'NONE',  ( 45.86712807150329496, 61.70051614449766220, 5.649768623646139964 ) ) ;
#8041 = DIRECTION ( 'NONE',  ( 0.1045284632676635322, -0.9945218953682722907, 0.000000000000000000 ) ) ;
#8042 = DIRECTION ( 'NONE',  ( 1.000000000000000000, 1.387778780781445676E-16, -0.000000000000000000 ) ) ;
#8043 = VECTOR ( 'NONE', #10984, 1000.000000000000000 ) ;
#8044 = EDGE_LOOP ( 'NONE', ( #19305, #8387, #1216, #13473 ) ) ;
#8045 = CARTESIAN_POINT ( 'NONE',  ( 1.000000000000000444, -15.10102051443364246, 9.000000000000000000 ) ) ;
#8046 = AXIS2_PLACEMENT_3D ( 'NONE', #14518, #1103, #17192 ) ;
#8047 = DIRECTION ( 'NONE',  ( -1.000000000000000000, 0.000000000000000000, 0.000000000000000000 ) ) ;
#8048 = VECTOR ( 'NONE', #171, 1000.000000000000000 ) ;
#8049 = CARTESIAN_POINT ( 'NONE',  ( -0.1481481481481481122, -4.797713218419819903, -1.000000000000000000 ) ) ;
#8050 = EDGE_CURVE ( 'NONE', #5143, #15934, #17460, .T. ) ;
#8051 = DIRECTION ( 'NONE',  ( 1.000000000000000000, 0.000000000000000000, 0.000000000000000000 ) ) ;
#8052 = ORIENTED_EDGE ( 'NONE', *, *, #12618, .F. ) ;
#8053 = DIRECTION ( 'NONE',  ( 1.000000000000000000, 0.000000000000000000, -0.000000000000000000 ) ) ;
#8054 = CARTESIAN_POINT ( 'NONE',  ( -20.63749999999999929, 0.000000000000000000, -4.424999999999999822 ) ) ;
#8055 = CARTESIAN_POINT ( 'NONE',  ( 44.28664221472220675, 63.09948385550240602, -1.832500667257165317 ) ) ;
#8056 = CARTESIAN_POINT ( 'NONE',  ( -14.99999999999999822, -19.99999999999999645, -23.00000000000000000 ) ) ;
#8057 = CARTESIAN_POINT ( 'NONE',  ( 44.03140696652192787, 47.19948385550240744, -4.306917132069425058 ) ) ;
#8058 = FACE_OUTER_BOUND ( 'NONE', #18957, .T. ) ;
#8059 = AXIS2_PLACEMENT_3D ( 'NONE', #4466, #13477, #8959 ) ;
#8060 = CARTESIAN_POINT ( 'NONE',  ( 45.31609314410960820, 62.30051614449766362, -6.485486291978072693 ) ) ;
#8061 = EDGE_CURVE ( 'NONE', #15612, #19390, #5170, .T. ) ;
#8062 = CARTESIAN_POINT ( 'NONE',  ( 53.50833635130544508, 61.30051614449766362, 4.867452303228181343 ) ) ;
#8063 = CIRCLE ( 'NONE', #8375, 0.5999999999999998668 ) ;
#8064 = EDGE_CURVE ( 'NONE', #12888, #9683, #19056, .T. ) ;
#8065 = CARTESIAN_POINT ( 'NONE',  ( 20.00000000000000000, -14.99999999999999289, -23.00000000000000000 ) ) ;
#8066 = DIRECTION ( 'NONE',  ( 1.000000000000000000, 0.000000000000000000, 0.000000000000000000 ) ) ;
#8067 = ORIENTED_EDGE ( 'NONE', *, *, #19379, .T. ) ;
#8068 = MECHANICAL_DESIGN_GEOMETRIC_PRESENTATION_REPRESENTATION (  '', ( #2780 ), #19415 ) ;
#8069 = ORIENTED_EDGE ( 'NONE', *, *, #15919, .T. ) ;
#8070 = FACE_BOUND ( 'NONE', #5648, .T. ) ;
#8071 = ORIENTED_EDGE ( 'NONE', *, *, #9921, .F. ) ;
#8072 = EDGE_CURVE ( 'NONE', #18910, #4701, #2148, .T. ) ;
#8073 = CARTESIAN_POINT ( 'NONE',  ( 4.086376210449952140, 2.103254844323300343, 3.500000000000000000 ) ) ;
#8074 = ORIENTED_EDGE ( 'NONE', *, *, #2152, .T. ) ;
#8075 = DIRECTION ( 'NONE',  ( -0.000000000000000000, -0.000000000000000000, -1.000000000000000000 ) ) ;
#8076 =( GEOMETRIC_REPRESENTATION_CONTEXT ( 3 ) GLOBAL_UNCERTAINTY_ASSIGNED_CONTEXT ( ( #16763 ) ) GLOBAL_UNIT_ASSIGNED_CONTEXT ( ( #18357, #3343, #7844 ) ) REPRESENTATION_CONTEXT ( 'NONE', 'WORKASPACE' ) );
#8077 = CARTESIAN_POINT ( 'NONE',  ( 55.94051828345050836, 49.79948385550240175, -4.345558710429103577 ) ) ;
#8078 = AXIS2_PLACEMENT_3D ( 'NONE', #10969, #16978, #5094 ) ;
#8079 = ORIENTED_EDGE ( 'NONE', *, *, #18997, .T. ) ;
#8080 = CARTESIAN_POINT ( 'NONE',  ( 6.533910050139696502, -2.950514251728084236, -5.110440592449055686 ) ) ;
#8081 = ORIENTED_EDGE ( 'NONE', *, *, #16962, .T. ) ;
#8082 = CARTESIAN_POINT ( 'NONE',  ( 52.57664461997811856, 53.59948385550240602, -8.007379884777229506 ) ) ;
#8083 = CARTESIAN_POINT ( 'NONE',  ( 4.086375874528100027, -2.103253014742892280, -3.499999999999999556 ) ) ;
#8084 = CARTESIAN_POINT ( 'NONE',  ( 45.90387839640214196, 64.69948385550240744, 5.676469297603166098 ) ) ;
#8085 = PLANE ( 'NONE',  #15416 ) ;
#8086 = DIRECTION ( 'NONE',  ( 0.000000000000000000, -1.000000000000000000, 8.673617379884035472E-16 ) ) ;
#8087 = MECHANICAL_DESIGN_GEOMETRIC_PRESENTATION_REPRESENTATION (  '', ( #4971 ), #12476 ) ;
#8088 = CARTESIAN_POINT ( 'NONE',  ( 42.63976443033212860, 58.00051614449765225, -0.02388180880514948964 ) ) ;
#8089 = EDGE_CURVE ( 'NONE', #8295, #13819, #9778, .T. ) ;
#8090 = CARTESIAN_POINT ( 'NONE',  ( 43.34962307344081012, 56.89948385550240317, 2.184720259617164650 ) ) ;
#8091 = CARTESIAN_POINT ( 'NONE',  ( -62.49999999999997158, 32.50000000000001421, 9.999999999999998224 ) ) ;
#8092 = DIRECTION ( 'NONE',  ( 0.000000000000000000, 0.000000000000000000, 1.000000000000000000 ) ) ;
#8093 = AXIS2_PLACEMENT_3D ( 'NONE', #10758, #9375, #15367 ) ;
#8094 = ORIENTED_EDGE ( 'NONE', *, *, #13270, .T. ) ;
#8095 = TOROIDAL_SURFACE ( 'NONE', #16277, 5.000000000000000000, 0.5999999999999999778 ) ;
#8096 = EDGE_LOOP ( 'NONE', ( #8198, #6119, #11453, #209 ) ) ;
#8097 = FACE_BOUND ( 'NONE', #11984, .T. ) ;
#8098 = CARTESIAN_POINT ( 'NONE',  ( 55.94051828345050836, 53.79948385550238754, -4.345558710429104465 ) ) ;
#8099 = PRESENTATION_LAYER_ASSIGNMENT (  '', '', ( #15624 ) ) ;
#8100 = ORIENTED_EDGE ( 'NONE', *, *, #6502, .F. ) ;
#8101 = VERTEX_POINT ( 'NONE', #8110 ) ;
#8102 = CARTESIAN_POINT ( 'NONE',  ( -0.9999999999999995559, -15.10102051443364246, 15.00000000000000355 ) ) ;
#8103 = ORIENTED_EDGE ( 'NONE', *, *, #2338, .T. ) ;
#8104 = CYLINDRICAL_SURFACE ( 'NONE', #364, 12.49999999999999645 ) ;
#8105 = EDGE_LOOP ( 'NONE', ( #8653, #7977, #11759, #17968 ) ) ;
#8106 = CIRCLE ( 'NONE', #8417, 1.000000000000000222 ) ;
#8107 = EDGE_CURVE ( 'NONE', #10123, #5600, #17149, .T. ) ;
#8108 = AXIS2_PLACEMENT_3D ( 'NONE', #11205, #12685, #6797 ) ;
#8109 = CARTESIAN_POINT ( 'NONE',  ( 52.25172492374522903, 47.59948385550239891, -7.007379884777225953 ) ) ;
#8110 = CARTESIAN_POINT ( 'NONE',  ( -17.85000000000000142, -19.99999999999999289, -23.00000000000000000 ) ) ;
#8111 = CARTESIAN_POINT ( 'NONE',  ( 44.88205777487401349, 59.80051614449766362, 3.688883143319584779 ) ) ;
#8112 = CARTESIAN_POINT ( 'NONE',  ( 0.000000000000000000, 0.000000000000000000, 0.000000000000000000 ) ) ;
#8113 = ADVANCED_FACE ( 'NONE', ( #12722 ), #16822, .T. ) ;
#8114 = FILL_AREA_STYLE_COLOUR ( '', #13331 ) ;
#8115 =( GEOMETRIC_REPRESENTATION_CONTEXT ( 3 ) GLOBAL_UNCERTAINTY_ASSIGNED_CONTEXT ( ( #4607 ) ) GLOBAL_UNIT_ASSIGNED_CONTEXT ( ( #13095, #19107, #13462 ) ) REPRESENTATION_CONTEXT ( 'NONE', 'WORKASPACE' ) );
#8116 = CARTESIAN_POINT ( 'NONE',  ( -11.75570504584937481, -36.18033988749900942, 9.000000000000000000 ) ) ;
#8117 = CARTESIAN_POINT ( 'NONE',  ( 50.02271294988505446, 60.50051614449766646, -8.000000000000001776 ) ) ;
#8118 = ORIENTED_EDGE ( 'NONE', *, *, #1133, .F. ) ;
#8119 = ORIENTED_EDGE ( 'NONE', *, *, #4651, .F. ) ;
#8120 = DIRECTION ( 'NONE',  ( -0.000000000000000000, -0.000000000000000000, 1.000000000000000000 ) ) ;
#8121 =( LENGTH_UNIT ( ) NAMED_UNIT ( * ) SI_UNIT ( .MILLI., .METRE. ) );
#8122 = VECTOR ( 'NONE', #9521, 1000.000000000000000 ) ;
#8123 = DIRECTION ( 'NONE',  ( -0.000000000000000000, 0.000000000000000000, -1.000000000000000000 ) ) ;
#8124 = CONTEXT_DEPENDENT_SHAPE_REPRESENTATION ( #272, #16368 ) ;
#8125 = ORIENTED_EDGE ( 'NONE', *, *, #5425, .T. ) ;
#8126 = CARTESIAN_POINT ( 'NONE',  ( 6.534838248920899595, -2.951765777552420644, -5.112608298763837489 ) ) ;
#8127 = FACE_OUTER_BOUND ( 'NONE', #11014, .T. ) ;
#8128 = VECTOR ( 'NONE', #1682, 1000.000000000000000 ) ;
#8129 = ORIENTED_EDGE ( 'NONE', *, *, #5020, .T. ) ;
#8130 = ADVANCED_FACE ( 'NONE', ( #15773 ), #12825, .F. ) ;
#8131 = CYLINDRICAL_SURFACE ( 'NONE', #1284, 6.080745460913608902 ) ;
#8132 = DIRECTION ( 'NONE',  ( 0.000000000000000000, 0.000000000000000000, 1.000000000000000000 ) ) ;
#8133 = DIRECTION ( 'NONE',  ( 1.000000000000000000, 0.000000000000000000, 0.000000000000000000 ) ) ;
#8134 = CIRCLE ( 'NONE', #15351, 6.080745460913608902 ) ;
#8135 = LINE ( 'NONE', #12354, #2345 ) ;
#8136 = LINE ( 'NONE', #12270, #14957 ) ;
#8137 = CARTESIAN_POINT ( 'NONE',  ( 48.07319477248768180, 46.59948385550239891, 6.007379884777225953 ) ) ;
#8138 = CIRCLE ( 'NONE', #10647, 4.000000000000000000 ) ;
#8139 = LINE ( 'NONE', #597, #681 ) ;
#8140 = CIRCLE ( 'NONE', #1290, 20.00000000000000000 ) ;
#8141 = CARTESIAN_POINT ( 'NONE',  ( 57.60143344285433642, 57.89948385550241028, -2.493737253992118319 ) ) ;
#8142 = CARTESIAN_POINT ( 'NONE',  ( 56.65037692655921120, 59.10051614449766078, 2.184720259617097593 ) ) ;
#8143 = AXIS2_PLACEMENT_3D ( 'NONE', #17205, #15725, #14237 ) ;
#8144 = DIRECTION ( 'NONE',  ( -0.000000000000000000, -0.000000000000000000, 1.000000000000000000 ) ) ;
#8145 = FACE_OUTER_BOUND ( 'NONE', #4776, .T. ) ;
#8146 =( NAMED_UNIT ( * ) SI_UNIT ( $, .STERADIAN. ) SOLID_ANGLE_UNIT ( ) );
#8147 = VERTEX_POINT ( 'NONE', #6545 ) ;
#8148 = CARTESIAN_POINT ( 'NONE',  ( -4.799999999999999822, 5.878304635907294211E-16, 0.000000000000000000 ) ) ;
#8149 = CARTESIAN_POINT ( 'NONE',  ( -0.1713913650100259145, 6.827405905246493187E-16, -5.575000000000000178 ) ) ;
#8150 = VECTOR ( 'NONE', #6841, 1000.000000000000000 ) ;
#8151 = AXIS2_PLACEMENT_3D ( 'NONE', #2709, #1034, #6997 ) ;
#8152 = CARTESIAN_POINT ( 'NONE',  ( 45.86712807150329496, 53.70051614449766220, 5.649768623646139964 ) ) ;
#8153 = CARTESIAN_POINT ( 'NONE',  ( -30.00000000000000000, -3.000000000000002665, 6.000000000000003553 ) ) ;
#8154 = CIRCLE ( 'NONE', #10665, 4.000000000000000000 ) ;
#8155 = DIRECTION ( 'NONE',  ( 0.000000000000000000, 1.000000000000000000, 0.000000000000000000 ) ) ;
#8156 = VERTEX_POINT ( 'NONE', #12625 ) ;
#8157 = DIRECTION ( 'NONE',  ( -1.000000000000000000, 0.000000000000000000, 0.000000000000000000 ) ) ;
#8158 = CARTESIAN_POINT ( 'NONE',  ( -1.249999999999997558, 0.000000000000000000, 0.000000000000000000 ) ) ;
#8159 = CARTESIAN_POINT ( 'NONE',  ( 22.00000000000000000, -20.00000000000000000, -20.00000000000000000 ) ) ;
#8160 = PRESENTATION_STYLE_ASSIGNMENT (( #17102 ) ) ;
#8161 = CARTESIAN_POINT ( 'NONE',  ( -3.680118525130244400, 2.494084732383327285, -0.3507732604232449702 ) ) ;
#8162 = CARTESIAN_POINT ( 'NONE',  ( 54.72065718078918906, 62.70051614449766220, -6.458785618021089192 ) ) ;
#8163 = AXIS2_PLACEMENT_3D ( 'NONE', #1466, #287, #6262 ) ;
#8164 = CARTESIAN_POINT ( 'NONE',  ( 55.08986747509849380, 63.20051614449766220, 3.727524721679155384 ) ) ;
#8165 = CARTESIAN_POINT ( 'NONE',  ( -17.32050807568879236, -10.00000000000004263, -9.000000000000000000 ) ) ;
#8166 = AXIS2_PLACEMENT_3D ( 'NONE', #10252, #5369, #9865 ) ;
#8167 = FACE_OUTER_BOUND ( 'NONE', #7314, .T. ) ;
#8168 = CIRCLE ( 'NONE', #7552, 0.5999999999999998668 ) ;
#8169 = ORIENTED_EDGE ( 'NONE', *, *, #6754, .T. ) ;
#8170 = ORIENTED_EDGE ( 'NONE', *, *, #17899, .T. ) ;
#8171 = VERTEX_POINT ( 'NONE', #765 ) ;
#8172 = CARTESIAN_POINT ( 'NONE',  ( -54.99999999999996447, -14.99999999999998579, 15.00000000000000000 ) ) ;
#8173 = ORIENTED_EDGE ( 'NONE', *, *, #417, .T. ) ;
#8174 = CARTESIAN_POINT ( 'NONE',  ( -57.64999999999994884, -14.99999999999998579, 10.00000000000000000 ) ) ;
#8175 = ORIENTED_EDGE ( 'NONE', *, *, #15633, .F. ) ;
#8176 = CYLINDRICAL_SURFACE ( 'NONE', #13784, 20.00000000000000000 ) ;
#8177 = EDGE_CURVE ( 'NONE', #15477, #7193, #6187, .T. ) ;
#8178 = CARTESIAN_POINT ( 'NONE',  ( 45.90387839640214196, 60.69948385550240033, 5.676469297603166098 ) ) ;
#8179 = ORIENTED_EDGE ( 'NONE', *, *, #4733, .T. ) ;
#8180 = CARTESIAN_POINT ( 'NONE',  ( 6.436591462021357124, -2.894509378375969000, -5.013437306331776533 ) ) ;
#8181 = AXIS2_PLACEMENT_3D ( 'NONE', #9458, #13868, #9547 ) ;
#8182 = EDGE_LOOP ( 'NONE', ( #5228, #18965, #6228, #19328 ) ) ;
#8183 = CARTESIAN_POINT ( 'NONE',  ( 52.62207051974839089, 54.39948385550241028, 7.992620115222770494 ) ) ;
#8184 = AXIS2_PLACEMENT_3D ( 'NONE', #4218, #8627, #8535 ) ;
#8185 = CARTESIAN_POINT ( 'NONE',  ( -74.99999999999997158, 1.000000000000000000, 6.000000000000000000 ) ) ;
#8186 = ADVANCED_FACE ( 'NONE', ( #6939 ), #12529, .F. ) ;
#8187 = PRODUCT_DEFINITION_SHAPE ( 'NONE', 'NONE',  #6742 ) ;
#8188 = CARTESIAN_POINT ( 'NONE',  ( 50.02271294988512551, 64.49948385550240459, 7.000000000000000888 ) ) ;
#8189 = DIRECTION ( 'NONE',  ( 0.000000000000000000, 0.000000000000000000, -1.000000000000000000 ) ) ;
#8190 = CARTESIAN_POINT ( 'NONE',  ( 4.071447262713890680, -4.041451884327386779, 0.000000000000000000 ) ) ;
#8191 = CARTESIAN_POINT ( 'NONE',  ( 55.96859303347802239, 60.80051614449764941, -4.306917132069484566 ) ) ;
#8192 = ADVANCED_FACE ( 'NONE', ( #17350 ), #3909, .F. ) ;
#8193 = CARTESIAN_POINT ( 'NONE',  ( 46.45491332379572924, 63.29948385550240175, -4.840751629271157874 ) ) ;
#8194 = EDGE_CURVE ( 'NONE', #7897, #8685, #14382, .T. ) ;
#8195 = CARTESIAN_POINT ( 'NONE',  ( 55.96859303347804371, 56.19948385550241454, 4.306917132069425946 ) ) ;
#8196 = CARTESIAN_POINT ( 'NONE',  ( 6.533910050139693837, -2.950514251728023840, 5.110440592449081443 ) ) ;
#8197 = CARTESIAN_POINT ( 'NONE',  ( 6.196878017913834746, -5.292377467571577121, -0.8333333333333331483 ) ) ;
#8198 = ORIENTED_EDGE ( 'NONE', *, *, #13469, .T. ) ;
#8199 = EDGE_CURVE ( 'NONE', #2892, #11964, #5762, .T. ) ;
#8200 = ORIENTED_EDGE ( 'NONE', *, *, #4256, .T. ) ;
#8201 = DIRECTION ( 'NONE',  ( -0.8090169943749430104, -0.5877852522924791323, 0.000000000000000000 ) ) ;
#8202 = CARTESIAN_POINT ( 'NONE',  ( 45.86712807150323812, 49.29948385550240175, -5.649768623646098220 ) ) ;
#8203 = VECTOR ( 'NONE', #14203, 1000.000000000000000 ) ;
#8204 = DIRECTION ( 'NONE',  ( 1.000000000000000000, 0.000000000000000000, 0.000000000000000000 ) ) ;
#8205 = ORIENTED_EDGE ( 'NONE', *, *, #16944, .F. ) ;
#8206 = ORIENTED_EDGE ( 'NONE', *, *, #10708, .F. ) ;
#8207 = CARTESIAN_POINT ( 'NONE',  ( -7.134732861515892033, -38.27090915285207018, 9.000000000000000000 ) ) ;
#8208 = EDGE_CURVE ( 'NONE', #13672, #590, #19222, .T. ) ;
#8209 = ADVANCED_FACE ( 'NONE', ( #2834 ), #19320, .F. ) ;
#8210 = ORIENTED_EDGE ( 'NONE', *, *, #3886, .F. ) ;
#8211 = LINE ( 'NONE', #12820, #18529 ) ;
#8212 = ORIENTED_EDGE ( 'NONE', *, *, #222, .F. ) ;
#8213 = CARTESIAN_POINT ( 'NONE',  ( 56.65037692655918988, 47.89948385550240317, -2.184720259617163762 ) ) ;
#8214 = CARTESIAN_POINT ( 'NONE',  ( 4.000000000000000000, 0.7924765000094659007, -0.05906175389889852662 ) ) ;
#8215 = AXIS2_PLACEMENT_3D ( 'NONE', #7589, #12191, #7681 ) ;
#8216 = CARTESIAN_POINT ( 'NONE',  ( 48.07319477248762496, 64.40051614449764372, -6.007379884777208190 ) ) ;
#8217 = CARTESIAN_POINT ( 'NONE',  ( -7.211304515372694901, -1.345319965580611843, -9.000000000000000000 ) ) ;
#8218 = CARTESIAN_POINT ( 'NONE',  ( 1.925929944387235853E-31, 15.00000000000001599, -15.00000000000000000 ) ) ;
#8219 = ORIENTED_EDGE ( 'NONE', *, *, #7417, .F. ) ;
#8220 = VERTEX_POINT ( 'NONE', #8602 ) ;
#8221 = CARTESIAN_POINT ( 'NONE',  ( 4.000000000000000000, -2.471525695159793035, -3.686886880705770864 ) ) ;
#8222 = CARTESIAN_POINT ( 'NONE',  ( -59.84999999999998721, 32.50000000000001421, 10.00000000000000000 ) ) ;
#8223 = ITEM_DEFINED_TRANSFORMATION ( 'NONE', 'NONE', #720,  #10359 ) ;
#8224 = ORIENTED_EDGE ( 'NONE', *, *, #8499, .F. ) ;
#8225 = CARTESIAN_POINT ( 'NONE',  ( -4.000000000000000000, -2.309401076758512694, -3.433295621305382461 ) ) ;
#8226 = CARTESIAN_POINT ( 'NONE',  ( -154.9999999999999716, -14.99999999999999645, -9.000000000000000000 ) ) ;
#8227 = ORIENTED_EDGE ( 'NONE', *, *, #11434, .T. ) ;
#8228 = DIRECTION ( 'NONE',  ( 0.000000000000000000, 1.000000000000000000, 0.000000000000000000 ) ) ;
#8229 = DIRECTION ( 'NONE',  ( -1.000000000000000000, 0.000000000000000000, 0.000000000000000000 ) ) ;
#8230 = CARTESIAN_POINT ( 'NONE',  ( 4.165266963751722784, 4.099263933823986683, 2.067493599750144616E-15 ) ) ;
#8231 = DIRECTION ( 'NONE',  ( 1.000000000000000000, 0.000000000000000000, 0.000000000000000000 ) ) ;
#8232 = DIRECTION ( 'NONE',  ( 0.000000000000000000, 0.000000000000000000, 1.000000000000000000 ) ) ;
#8233 = CARTESIAN_POINT ( 'NONE',  ( 54.09612160359786515, 63.69948385550240744, -5.676469297603166098 ) ) ;
#8234 = ADVANCED_BREP_SHAPE_REPRESENTATION ( '', ( #14979, #10359 ), #1557 ) ;
#8235 = CARTESIAN_POINT ( 'NONE',  ( -0.9996874511566102850, -0.02500000000000036915, 9.000000000000000000 ) ) ;
#8236 = CARTESIAN_POINT ( 'NONE',  ( 56.65037692655918988, 45.89948385550240317, -2.184720259617163762 ) ) ;
#8237 = CARTESIAN_POINT ( 'NONE',  ( 45.90387839640208512, 64.30051614449766362, -5.676469297603124353 ) ) ;
#8238 = DIRECTION ( 'NONE',  ( 1.000000000000000000, 0.000000000000000000, 0.000000000000000000 ) ) ;
#8239 = DIRECTION ( 'NONE',  ( 0.000000000000000000, 0.000000000000000000, 1.000000000000000000 ) ) ;
#8240 = ADVANCED_FACE ( 'NONE', ( #10162 ), #17542, .F. ) ;
#8241 = DIRECTION ( 'NONE',  ( -9.710251638871368927E-17, -5.969973981896232516E-17, -0.9999999999999997780 ) ) ;
#8242 = ORIENTED_EDGE ( 'NONE', *, *, #17259, .T. ) ;
#8243 = CARTESIAN_POINT ( 'NONE',  ( 8.500000000000000000, -2.886751345948133984, -5.000000000000000000 ) ) ;
#8244 = EDGE_CURVE ( 'NONE', #18044, #18478, #1158, .T. ) ;
#8245 = DIRECTION ( 'NONE',  ( 0.000000000000000000, 0.000000000000000000, -1.000000000000000000 ) ) ;
#8246 = CARTESIAN_POINT ( 'NONE',  ( 42.63976443033212149, 50.00051614449765935, -0.02388180880514948964 ) ) ;
#8247 = AXIS2_PLACEMENT_3D ( 'NONE', #620, #2005, #13597 ) ;
#8248 = CARTESIAN_POINT ( 'NONE',  ( 19.76107906696393357, -23.08216711247132835, -9.000000000000000000 ) ) ;
#8249 = CARTESIAN_POINT ( 'NONE',  ( 52.80949999999998568, 0.000000000000000000, 0.000000000000000000 ) ) ;
#8250 = LINE ( 'NONE', #810, #10860 ) ;
#8251 = CARTESIAN_POINT ( 'NONE',  ( -20.00000000000000000, -19.99999999999999289, -23.00000000000000000 ) ) ;
#8252 = CARTESIAN_POINT ( 'NONE',  ( 1.249999999999997558, 0.000000000000000000, -4.424999999999999822 ) ) ;
#8253 = CARTESIAN_POINT ( 'NONE',  ( -74.99999999999997158, 40.00000000000001421, 10.00000000000000000 ) ) ;
#8254 = CARTESIAN_POINT ( 'NONE',  ( 50.02271294988512551, 48.49948385550240459, 7.000000000000000888 ) ) ;
#8255 = CARTESIAN_POINT ( 'NONE',  ( 0.000000000000000000, -0.8865213383406694847, 1.535500000000001419 ) ) ;
#8256 = CARTESIAN_POINT ( 'NONE',  ( 56.79116909180255135, 45.79948385550240886, -4.963592699179005585 ) ) ;
#8257 = CARTESIAN_POINT ( 'NONE',  ( 48.02776887271750184, 63.60051614449764656, 5.992620115222795363 ) ) ;
#8258 = PLANE ( 'NONE',  #13503 ) ;
#8259 = CARTESIAN_POINT ( 'NONE',  ( 6.541171370350062020, -2.986177670315871335, 5.112746295475706582 ) ) ;
#8260 = AXIS2_PLACEMENT_3D ( 'NONE', #7758, #9416, #9316 ) ;
#8261 = ORIENTED_EDGE ( 'NONE', *, *, #2195, .F. ) ;
#8262 = VERTEX_POINT ( 'NONE', #19120 ) ;
#8263 = VERTEX_POINT ( 'NONE', #17734 ) ;
#8264 = LINE ( 'NONE', #827, #15312 ) ;
#8265 = ORIENTED_EDGE ( 'NONE', *, *, #16517, .T. ) ;
#8266 = CARTESIAN_POINT ( 'NONE',  ( 4.158806752148102248, -2.089318365061878513, 3.500000000000000000 ) ) ;
#8267 = VERTEX_POINT ( 'NONE', #17935 ) ;
#8268 = DIRECTION ( 'NONE',  ( 0.000000000000000000, 0.000000000000000000, 1.000000000000000000 ) ) ;
#8269 = CARTESIAN_POINT ( 'NONE',  ( 52.25172492374522903, 57.59948385550240602, -7.007379884777227730 ) ) ;
#8270 = ORIENTED_EDGE ( 'NONE', *, *, #1010, .F. ) ;
#8271 = CARTESIAN_POINT ( 'NONE',  ( -15.51323935927264586, -32.62297130559655045, 9.000000000000000000 ) ) ;
#8272 = ORIENTED_EDGE ( 'NONE', *, *, #16352, .T. ) ;
#8273 = CARTESIAN_POINT ( 'NONE',  ( 47.37792948025162332, 53.39948385550241028, -7.992620115222770494 ) ) ;
#8274 = AXIS2_PLACEMENT_3D ( 'NONE', #8032, #317, #17079 ) ;
#8275 = LINE ( 'NONE', #9461, #6083 ) ;
#8276 = CARTESIAN_POINT ( 'NONE',  ( 44.28664221472220675, 51.09948385550240602, -1.832500667257165317 ) ) ;
#8277 = CARTESIAN_POINT ( 'NONE',  ( 4.030867648404937498, 3.732851566701761659, 0.5345114293584584120 ) ) ;
#8278 = CARTESIAN_POINT ( 'NONE',  ( 4.114405500665258231, -4.051151509359434577, 3.301207616706364010E-16 ) ) ;
#8279 = CARTESIAN_POINT ( 'NONE',  ( 44.05948171654945611, 62.20051614449764799, -4.345558710429044069 ) ) ;
#8280 = AXIS2_PLACEMENT_3D ( 'NONE', #17907, #143, #53 ) ;
#8281 = CARTESIAN_POINT ( 'NONE',  ( 44.88205777487398507, 65.19948385550240744, -3.688883143319540814 ) ) ;
#8282 = CARTESIAN_POINT ( 'NONE',  ( 49.97728705011488159, 59.49948385550240459, -7.000000000000000888 ) ) ;
#8283 = CARTESIAN_POINT ( 'NONE',  ( 6.527192678185834929, -2.941622124011297412, 5.095038975455882913 ) ) ;
#8284 = DIRECTION ( 'NONE',  ( 0.000000000000000000, 0.5000000000000018874, 0.8660254037844375974 ) ) ;
#8285 = ADVANCED_FACE ( 'NONE', ( #8889 ), #4195, .F. ) ;
#8286 = ORIENTED_EDGE ( 'NONE', *, *, #1010, .T. ) ;
#8287 = AXIS2_PLACEMENT_3D ( 'NONE', #14110, #12937, #11162 ) ;
#8288 = ORIENTED_EDGE ( 'NONE', *, *, #3081, .T. ) ;
#8289 = DIRECTION ( 'NONE',  ( 0.000000000000000000, 1.000000000000000000, -1.224646799147353207E-16 ) ) ;
#8290 = ORIENTED_EDGE ( 'NONE', *, *, #5259, .F. ) ;
#8291 = CIRCLE ( 'NONE', #11410, 1.000000000000000444 ) ;
#8292 = CARTESIAN_POINT ( 'NONE',  ( 49.97728705011488159, 61.49948385550240459, -7.000000000000000888 ) ) ;
#8293 = CYLINDRICAL_SURFACE ( 'NONE', #12174, 20.00000000000000000 ) ;
#8294 = VERTEX_POINT ( 'NONE', #4495 ) ;
#8295 = VERTEX_POINT ( 'NONE', #10070 ) ;
#8296 = LINE ( 'NONE', #14565, #15854 ) ;
#8297 = VERTEX_POINT ( 'NONE', #13402 ) ;
#8298 = CARTESIAN_POINT ( 'NONE',  ( 44.03140696652198471, 63.80051614449764941, 4.306917132069485454 ) ) ;
#8299 = ORIENTED_EDGE ( 'NONE', *, *, #14682, .F. ) ;
#8300 = ADVANCED_FACE ( 'NONE', ( #11930 ), #11636, .T. ) ;
#8301 = CARTESIAN_POINT ( 'NONE',  ( 75.00000000000000000, 40.00000000000000000, -10.00000000000000000 ) ) ;
#8302 = CARTESIAN_POINT ( 'NONE',  ( 1.267864665251833278E-11, -20.00000000000000000, 9.000000000000000000 ) ) ;
#8303 = ADVANCED_FACE ( 'NONE', ( #15966 ), #7426, .T. ) ;
#8304 = CARTESIAN_POINT ( 'NONE',  ( 54.13287192849671214, 44.70051614449766220, -5.649768623646139964 ) ) ;
#8305 = DIRECTION ( 'NONE',  ( -0.4999999999999933942, -0.8660254037844425934, 0.000000000000000000 ) ) ;
#8306 = CARTESIAN_POINT ( 'NONE',  ( 49.97728705011488159, 45.49948385550240459, -7.000000000000000888 ) ) ;
#8307 = CARTESIAN_POINT ( 'NONE',  ( -74.99999999999997158, 20.00000000000001421, 15.00000000000000000 ) ) ;
#8308 = EDGE_CURVE ( 'NONE', #6920, #4928, #2553, .T. ) ;
#8309 = EDGE_CURVE ( 'NONE', #18696, #8779, #6194, .T. ) ;
#8310 = ORIENTED_EDGE ( 'NONE', *, *, #15693, .F. ) ;
#8311 = ORIENTED_EDGE ( 'NONE', *, *, #772, .F. ) ;
#8312 = CARTESIAN_POINT ( 'NONE',  ( 4.000000000000000888, 0.8228435280416209752, -3.430609588141487976 ) ) ;
#8313 = SURFACE_SIDE_STYLE ('',( #15581 ) ) ;
#8314 = FACE_OUTER_BOUND ( 'NONE', #13167, .T. ) ;
#8315 = MECHANICAL_DESIGN_GEOMETRIC_PRESENTATION_REPRESENTATION (  '', ( #10189 ), #19319 ) ;
#8316 = DIRECTION ( 'NONE',  ( -1.000000000000000000, 1.734723475976806848E-16, 0.000000000000000000 ) ) ;
#8317 = ITEM_DEFINED_TRANSFORMATION ( 'NONE', 'NONE', #6665,  #10359 ) ;
#8318 = VERTEX_POINT ( 'NONE', #16163 ) ;
#8319 = CARTESIAN_POINT ( 'NONE',  ( -154.9999999999999716, -14.99999999999999645, 6.499999999999999112 ) ) ;
#8320 = EDGE_CURVE ( 'NONE', #7574, #4179, #1351, .T. ) ;
#8322 = ADVANCED_FACE ( 'NONE', ( #10257 ), #10254, .F. ) ;
#8321 = ORIENTED_EDGE ( 'NONE', *, *, #16166, .T. ) ;
#8323 = CIRCLE ( 'NONE', #16796, 1.000000000000000222 ) ;
#8324 = ADVANCED_FACE ( 'NONE', ( #16259 ), #8798, .F. ) ;
#8325 = CARTESIAN_POINT ( 'NONE',  ( 0.000000000000000000, 3.755786496842903495E-16, 3.500000000000000000 ) ) ;
#8326 = FACE_BOUND ( 'NONE', #2658, .T. ) ;
#8327 = PLANE ( 'NONE',  #2040 ) ;
#8328 = FACE_OUTER_BOUND ( 'NONE', #10320, .T. ) ;
#8329 = CIRCLE ( 'NONE', #7707, 1.000000000000000888 ) ;
#8330 = CARTESIAN_POINT ( 'NONE',  ( 51.97223112728254790, 48.39948385550240317, 5.992620115222778487 ) ) ;
#8331 = DIRECTION ( 'NONE',  ( -1.000000000000000000, 0.000000000000000000, 0.000000000000000000 ) ) ;
#8332 = CARTESIAN_POINT ( 'NONE',  ( 58.41169779390614281, 63.99948385550241170, -0.02388180880523160798 ) ) ;
#8333 = CARTESIAN_POINT ( 'NONE',  ( 56.66441430157294690, 62.90051614449765083, -2.141517661632166281 ) ) ;
#8334 = DIRECTION ( 'NONE',  ( 0.000000000000000000, -1.224646799147353207E-16, 1.000000000000000000 ) ) ;
#8335 = CARTESIAN_POINT ( 'NONE',  ( 6.541171661047875396, 5.920857802016174176, 0.02973393389964464062 ) ) ;
#8336 = CIRCLE ( 'NONE', #5216, 24.99999999999999289 ) ;
#8337 = VERTEX_POINT ( 'NONE', #5859 ) ;
#8338 = CARTESIAN_POINT ( 'NONE',  ( 1.000000000000000444, -15.10102051443364246, 15.00000000000000355 ) ) ;
#8339 = PRODUCT_DEFINITION_SHAPE ( 'NONE', 'NONE',  #19436 ) ;
#8340 = DIRECTION ( 'NONE',  ( -1.000000000000000000, 0.000000000000000000, 0.000000000000000000 ) ) ;
#8341 = CARTESIAN_POINT ( 'NONE',  ( 44.05948171654945611, 50.20051614449765509, -4.345558710429044069 ) ) ;
#8342 = CIRCLE ( 'NONE', #12115, 2.447112362156698140 ) ;
#8343 = DIRECTION ( 'NONE',  ( 0.000000000000000000, 0.000000000000000000, 1.000000000000000000 ) ) ;
#8344 = CARTESIAN_POINT ( 'NONE',  ( 5.000000000000003553, -20.00000000000000000, -8.999999999999998224 ) ) ;
#8345 = ORIENTED_EDGE ( 'NONE', *, *, #17562, .T. ) ;
#8346 = CARTESIAN_POINT ( 'NONE',  ( 4.033901012035946643, -3.740908793664254883, 0.5205559028926849408 ) ) ;
#8347 = AXIS2_PLACEMENT_3D ( 'NONE', #17957, #4515, #10474 ) ;
#8348 = DIRECTION ( 'NONE',  ( -1.000000000000000000, 0.000000000000000000, -0.000000000000000000 ) ) ;
#8349 = ADVANCED_FACE ( 'NONE', ( #17831 ), #16361, .T. ) ;
#8350 = DIRECTION ( 'NONE',  ( -9.251858538542972814E-17, -1.000000000000000000, 0.000000000000000000 ) ) ;
#8351 = CARTESIAN_POINT ( 'NONE',  ( 50.02271294988512551, 50.49948385550240459, 7.000000000000000888 ) ) ;
#8352 = CARTESIAN_POINT ( 'NONE',  ( 73.00000000000002842, -3.000000000000000000, -5.999999999999998224 ) ) ;
#8353 = CARTESIAN_POINT ( 'NONE',  ( 42.38452918213188525, 47.09948385550240602, -2.450534656007040013 ) ) ;
#8354 = FACE_OUTER_BOUND ( 'NONE', #985, .T. ) ;
#8355 = EDGE_CURVE ( 'NONE', #4952, #9732, #4000, .T. ) ;
#8356 = CARTESIAN_POINT ( 'NONE',  ( 48.07319477248762496, 64.40051614449764372, -6.007379884777208190 ) ) ;
#8357 = DIRECTION ( 'NONE',  ( 0.000000000000000000, 0.000000000000000000, 1.000000000000000000 ) ) ;
#8358 = CARTESIAN_POINT ( 'NONE',  ( 8.500000000000000000, 4.898587196589412829E-16, -4.000000000000000000 ) ) ;
#8359 = VERTEX_POINT ( 'NONE', #12025 ) ;
#8360 = AXIS2_PLACEMENT_3D ( 'NONE', #8841, #17681, #19170 ) ;
#8361 = EDGE_LOOP ( 'NONE', ( #14388, #9636, #9561, #12686 ) ) ;
#8362 = FACE_OUTER_BOUND ( 'NONE', #11445, .T. ) ;
#8363 = AXIS2_PLACEMENT_3D ( 'NONE', #2718, #2807, #4173 ) ;
#8364 = VERTEX_POINT ( 'NONE', #13874 ) ;
#8365 = CARTESIAN_POINT ( 'NONE',  ( 4.052432342741587590, 1.393590342655181891, 3.567979436357439305 ) ) ;
#8366 = VERTEX_POINT ( 'NONE', #10545 ) ;
#8367 = FACE_OUTER_BOUND ( 'NONE', #9448, .T. ) ;
#8368 = CARTESIAN_POINT ( 'NONE',  ( 54.13287192849676188, 58.29948385550240175, 5.649768623646098220 ) ) ;
#8369 = EDGE_LOOP ( 'NONE', ( #12332, #10004, #10394, #3669 ) ) ;
#8370 = CYLINDRICAL_SURFACE ( 'NONE', #8677, 0.7500000000000000000 ) ;
#8371 = ORIENTED_EDGE ( 'NONE', *, *, #1677, .F. ) ;
#8372 = AXIS2_PLACEMENT_3D ( 'NONE', #15117, #7277, #4336 ) ;
#8373 = CARTESIAN_POINT ( 'NONE',  ( 54.72065718078924590, 58.29948385550240886, 6.458785618021043895 ) ) ;
#8374 = CARTESIAN_POINT ( 'NONE',  ( -57.64999999999994884, -14.99999999999998579, 15.00000000000000000 ) ) ;
#8375 = AXIS2_PLACEMENT_3D ( 'NONE', #12851, #17669, #8238 ) ;
#8376 = CARTESIAN_POINT ( 'NONE',  ( 44.88205777487398507, 53.19948385550240744, -3.688883143319540814 ) ) ;
#8377 = LINE ( 'NONE', #11702, #5399 ) ;
#8378 = CARTESIAN_POINT ( 'NONE',  ( 4.142654963991854622, -4.070796997468703715, 6.968404583626299416E-17 ) ) ;
#8379 = CARTESIAN_POINT ( 'NONE',  ( 42.39856655714564226, 46.10051614449766078, -2.493737253992044156 ) ) ;
#8380 = CARTESIAN_POINT ( 'NONE',  ( 56.30877334542961421, 63.99948385550241170, -0.02388180880520959434 ) ) ;
#8381 = CARTESIAN_POINT ( 'NONE',  ( -31.74999999999995737, 2.449293598294707893E-16, -2.000000000000000888 ) ) ;
#8382 = CARTESIAN_POINT ( 'NONE',  ( 2.449293598294706513E-15, -20.00000000000000000, 9.000000000000000000 ) ) ;
#8383 = ORIENTED_EDGE ( 'NONE', *, *, #2638, .F. ) ;
#8384 = B_SPLINE_CURVE_WITH_KNOTS ( 'NONE', 3,
 ( #4369, #4470, #7110, #4271, #10332, #13191 ),
 .UNSPECIFIED., .F., .F.,
 ( 4, 2, 4 ),
 ( 9.961792871202292917E-20, 0.002086519881787258883, 0.004173039763574517766 ),
 .UNSPECIFIED. ) ;
#8385 = VERTEX_POINT ( 'NONE', #18026 ) ;
#8386 = DIRECTION ( 'NONE',  ( -1.000000000000000000, -0.000000000000000000, -0.000000000000000000 ) ) ;
#8387 = ORIENTED_EDGE ( 'NONE', *, *, #1633, .F. ) ;
#8388 = PRESENTATION_LAYER_ASSIGNMENT (  '', '', ( #18133 ) ) ;
#8389 = AXIS2_PLACEMENT_3D ( 'NONE', #7242, #19230, #8899 ) ;
#8390 = CARTESIAN_POINT ( 'NONE',  ( 44.03140696652192787, 59.19948385550238612, -4.306917132069425058 ) ) ;
#8391 = DIRECTION ( 'NONE',  ( 1.000000000000000000, 0.000000000000000000, -0.000000000000000000 ) ) ;
#8392 = ORIENTED_EDGE ( 'NONE', *, *, #3820, .F. ) ;
#8393 = ORIENTED_EDGE ( 'NONE', *, *, #2084, .F. ) ;
#8394 = DIRECTION ( 'NONE',  ( 1.000000000000000000, 0.000000000000000000, 0.000000000000000000 ) ) ;
#8395 = MANIFOLD_SOLID_BREP ( 'FlangeHexFillet', #3665 ) ;
#8396 = VERTEX_POINT ( 'NONE', #13507 ) ;
#8397 = PRESENTATION_LAYER_ASSIGNMENT (  '', '', ( #12237 ) ) ;
#8398 = DIRECTION ( 'NONE',  ( 0.000000000000000000, -1.000000000000000000, 8.673617379884035472E-16 ) ) ;
#8399 = EDGE_LOOP ( 'NONE', ( #7975, #17559, #3009, #12035, #8494 ) ) ;
#8400 = CARTESIAN_POINT ( 'NONE',  ( 44.05948171654949874, 50.79948385550238754, 4.345558710429105354 ) ) ;
#8401 = CARTESIAN_POINT ( 'NONE',  ( -72.99999999999997158, -1.000000000000000000, -5.999999999999998224 ) ) ;
#8402 = CARTESIAN_POINT ( 'NONE',  ( 42.63976443033212860, 50.00051614449766646, -0.02388180880514948964 ) ) ;
#8403 = CARTESIAN_POINT ( 'NONE',  ( 0.1085714285714285687, -3.798448662927795372, -0.8000000000000000444 ) ) ;
#8404 =( GEOMETRIC_REPRESENTATION_CONTEXT ( 3 ) GLOBAL_UNCERTAINTY_ASSIGNED_CONTEXT ( ( #9109 ) ) GLOBAL_UNIT_ASSIGNED_CONTEXT ( ( #18621, #2139, #4885 ) ) REPRESENTATION_CONTEXT ( 'NONE', 'WORKASPACE' ) );
#8405 = AXIS2_PLACEMENT_3D ( 'NONE', #9850, #17235, #9949 ) ;
#8406 = DIRECTION ( 'NONE',  ( 0.000000000000000000, 1.000000000000000000, 0.000000000000000000 ) ) ;
#8407 = DIRECTION ( 'NONE',  ( 0.9781476007338055778, 0.2079116908177597867, 0.000000000000000000 ) ) ;
#8408 = VERTEX_POINT ( 'NONE', #13595 ) ;
#8409 = ORIENTED_EDGE ( 'NONE', *, *, #9328, .F. ) ;
#8410 = CARTESIAN_POINT ( 'NONE',  ( 3.973514160553461849, 2.741076955031360285, 2.383932505289871884 ) ) ;
#8411 = SURFACE_STYLE_USAGE ( .BOTH. , #9685 ) ;
#8412 = CARTESIAN_POINT ( 'NONE',  ( 75.00000000000002842, -39.99999999999998579, -10.00000000000000000 ) ) ;
#8413 = CARTESIAN_POINT ( 'NONE',  ( -62.49999999999997158, 32.50000000000001421, 15.00000000000000178 ) ) ;
#8414 = CONTEXT_DEPENDENT_SHAPE_REPRESENTATION ( #3031, #19361 ) ;
#8415 = ORIENTED_EDGE ( 'NONE', *, *, #301, .F. ) ;
#8416 = DIRECTION ( 'NONE',  ( 1.000000000000000000, 0.000000000000000000, -0.000000000000000000 ) ) ;
#8417 = AXIS2_PLACEMENT_3D ( 'NONE', #12301, #250, #9253 ) ;
#8418 = AXIS2_PLACEMENT_3D ( 'NONE', #11690, #2703, #8655 ) ;
#8419 = ORIENTED_EDGE ( 'NONE', *, *, #11783, .F. ) ;
#8420 = VERTEX_POINT ( 'NONE', #3400 ) ;
#8421 = EDGE_CURVE ( 'NONE', #1266, #12888, #3577, .T. ) ;
#8422 = DIRECTION ( 'NONE',  ( 0.000000000000000000, 0.000000000000000000, -1.000000000000000000 ) ) ;
#8423 =( GEOMETRIC_REPRESENTATION_CONTEXT ( 3 ) GLOBAL_UNCERTAINTY_ASSIGNED_CONTEXT ( ( #16383 ) ) GLOBAL_UNIT_ASSIGNED_CONTEXT ( ( #13001, #19007, #6924 ) ) REPRESENTATION_CONTEXT ( 'NONE', 'WORKASPACE' ) );
#8424 = CARTESIAN_POINT ( 'NONE',  ( 4.071447262713888016, 4.041451884327382338, 0.000000000000000000 ) ) ;
#8425 = CARTESIAN_POINT ( 'NONE',  ( 49.97728705011488870, 65.49948385550240459, -6.000000000000000888 ) ) ;
#8426 = CARTESIAN_POINT ( 'NONE',  ( -99.99999999999997158, -23.00000000000000711, -10.00000000000000178 ) ) ;
#8427 = EDGE_CURVE ( 'NONE', #9042, #3326, #3125, .T. ) ;
#8428 = MANIFOLD_SOLID_BREP ( 'Mirror3', #2102 ) ;
#8429 = CARTESIAN_POINT ( 'NONE',  ( 2.449293598294706513E-15, -20.00000000000000000, -9.000000000000000000 ) ) ;
#8430 = CARTESIAN_POINT ( 'NONE',  ( 46.49166364869460466, 52.69948385550240744, 4.867452303228209765 ) ) ;
#8431 = LINE ( 'NONE', #14409, #19183 ) ;
#8432 = CARTESIAN_POINT ( 'NONE',  ( 43.20883090819745576, 64.79948385550240175, 4.963592699179006473 ) ) ;
#8433 = VECTOR ( 'NONE', #9452, 1000.000000000000000 ) ;
#8434 = CARTESIAN_POINT ( 'NONE',  ( 50.02271294988505446, 64.50051614449765225, -7.000000000000000888 ) ) ;
#8435 = EDGE_CURVE ( 'NONE', #10530, #16860, #13686, .T. ) ;
#8436 = AXIS2_PLACEMENT_3D ( 'NONE', #14733, #7386, #15198 ) ;
#8437 = EDGE_CURVE ( 'NONE', #12240, #5733, #16744, .T. ) ;
#8438 = DIRECTION ( 'NONE',  ( 0.000000000000000000, 8.673617379884036458E-16, 1.000000000000000000 ) ) ;
#8439 = CARTESIAN_POINT ( 'NONE',  ( 6.204460410672268722, 3.831267809383005041, -3.364049496745006529 ) ) ;
#8440 = DIRECTION ( 'NONE',  ( 1.000000000000000000, 0.000000000000000000, 0.000000000000000000 ) ) ;
#8441 = AXIS2_PLACEMENT_3D ( 'NONE', #2687, #4331, #8639 ) ;
#8442 = ORIENTED_EDGE ( 'NONE', *, *, #16287, .F. ) ;
#8443 = CARTESIAN_POINT ( 'NONE',  ( -2.756197834950067094, -3.027510591568735254, -3.223146290109809797 ) ) ;
#8444 = LINE ( 'NONE', #14424, #11884 ) ;
#8445 = CARTESIAN_POINT ( 'NONE',  ( 50.02271294988505446, 52.50051614449765935, -7.000000000000000888 ) ) ;
#8446 = VECTOR ( 'NONE', #12260, 1000.000000000000000 ) ;
#8447 = EDGE_CURVE ( 'NONE', #18672, #468, #17869, .T. ) ;
#8448 = CARTESIAN_POINT ( 'NONE',  ( 0.000000000000000000, 0.5192545390863916310, -1.000000000000000000 ) ) ;
#8449 = EDGE_CURVE ( 'NONE', #15433, #16449, #6624, .T. ) ;
#8450 = CARTESIAN_POINT ( 'NONE',  ( 55.41777406314699306, 44.91366546079681399, -4.999999999999999112 ) ) ;
#8451 = EDGE_LOOP ( 'NONE', ( #15084, #2250, #17992, #10025 ) ) ;
#8452 = CARTESIAN_POINT ( 'NONE',  ( 3.961551342853522950, -3.742715940867789026, 0.5174258321190450260 ) ) ;
#8453 = LINE ( 'NONE', #14433, #18942 ) ;
#8454 = CARTESIAN_POINT ( 'NONE',  ( 2.742827927723449299, 3.035229711104609596, -3.433252694550591233 ) ) ;
#8455 = CARTESIAN_POINT ( 'NONE',  ( 55.94051828345050836, 53.79948385550238754, -4.345558710429104465 ) ) ;
#8456 = AXIS2_PLACEMENT_3D ( 'NONE', #2332, #13091, #8284 ) ;
#8457 = CARTESIAN_POINT ( 'NONE',  ( 20.00000000000000000, -14.99999999999999289, -23.00000000000000000 ) ) ;
#8458 = CARTESIAN_POINT ( 'NONE',  ( 50.02271294988513972, 46.49948385550240459, 8.000000000000001776 ) ) ;
#8459 = FILL_AREA_STYLE_COLOUR ( '', #14125 ) ;
#8460 = CARTESIAN_POINT ( 'NONE',  ( 54.13287192849671214, 46.70051614449766220, -5.649768623646139964 ) ) ;
#8461 = DIRECTION ( 'NONE',  ( 0.000000000000000000, 0.000000000000000000, -1.000000000000000000 ) ) ;
#8462 = CARTESIAN_POINT ( 'NONE',  ( -8.134732861516020819, -1.729090847147989773, -9.000000000000000000 ) ) ;
#8463 = AXIS2_PLACEMENT_3D ( 'NONE', #5100, #2065, #12547 ) ;
#8464 = ORIENTED_EDGE ( 'NONE', *, *, #4133, .T. ) ;
#8465 = CIRCLE ( 'NONE', #11903, 20.00000000000000000 ) ;
#8466 = ORIENTED_EDGE ( 'NONE', *, *, #16120, .T. ) ;
#8467 = CARTESIAN_POINT ( 'NONE',  ( 2.449293598294706513E-15, -20.00000000000000000, 9.000000000000000000 ) ) ;
#8468 = ORIENTED_EDGE ( 'NONE', *, *, #5310, .F. ) ;
#8469 = B_SPLINE_CURVE_WITH_KNOTS ( 'NONE', 3,
 ( #5499, #10005, #5601, #13336, #11573 ),
 .UNSPECIFIED., .F., .F.,
 ( 4, 1, 4 ),
 ( 0.000000000000000000, 0.002309401076758505356, 0.004618802153517010713 ),
 .UNSPECIFIED. ) ;
#8470 = CARTESIAN_POINT ( 'NONE',  ( 6.244297270354683960, 1.802013835206515036E-11, 5.105276777067893512 ) ) ;
#8471 = CIRCLE ( 'NONE', #10338, 4.872650870659752442 ) ;
#8472 = VERTEX_POINT ( 'NONE', #11029 ) ;
#8473 = DIRECTION ( 'NONE',  ( 1.000000000000000000, 0.000000000000000000, 0.000000000000000000 ) ) ;
#8474 = CARTESIAN_POINT ( 'NONE',  ( 43.34962307344081012, 58.89948385550241028, 2.184720259617164650 ) ) ;
#8475 = ORIENTED_EDGE ( 'NONE', *, *, #11067, .T. ) ;
#8476 = EDGE_CURVE ( 'NONE', #14776, #7333, #860, .T. ) ;
#8477 = DIRECTION ( 'NONE',  ( 0.000000000000000000, 0.000000000000000000, 1.000000000000000000 ) ) ;
#8478 = ORIENTED_EDGE ( 'NONE', *, *, #11659, .F. ) ;
#8479 = CARTESIAN_POINT ( 'NONE',  ( 56.81924384183011512, 56.19948385550240744, 4.924951120819313743 ) ) ;
#8480 = CIRCLE ( 'NONE', #2859, 2.649999999999987477 ) ;
#8481 = DIRECTION ( 'NONE',  ( -0.000000000000000000, -0.000000000000000000, 1.000000000000000000 ) ) ;
#8482 = CARTESIAN_POINT ( 'NONE',  ( 49.97728705011488870, 49.49948385550241170, -6.000000000000000888 ) ) ;
#8483 = EDGE_CURVE ( 'NONE', #9166, #8991, #2125, .T. ) ;
#8484 = DIRECTION ( 'NONE',  ( -0.000000000000000000, -0.000000000000000000, -1.000000000000000000 ) ) ;
#8485 = CARTESIAN_POINT ( 'NONE',  ( 8.500000000000000000, 2.886751345948123770, -5.000000000000000000 ) ) ;
#8486 = CIRCLE ( 'NONE', #14425, 12.49999999999999645 ) ;
#8487 = CIRCLE ( 'NONE', #10353, 20.00000000000000000 ) ;
#8488 = AXIS2_PLACEMENT_3D ( 'NONE', #17522, #19300, #17813 ) ;
#8489 = CARTESIAN_POINT ( 'NONE',  ( 57.60143344285435774, 45.10051614449766788, 2.493737253992045044 ) ) ;
#8490 = CARTESIAN_POINT ( 'NONE',  ( 48.02776887271750184, 49.60051614449766788, 5.992620115222795363 ) ) ;
#8491 = ADVANCED_BREP_SHAPE_REPRESENTATION ( '', ( #14815, #10359 ), #7771 ) ;
#8492 = CARTESIAN_POINT ( 'NONE',  ( 6.436591462021362453, -2.894509378375957009, 5.013437306331779197 ) ) ;
#8493 = CYLINDRICAL_SURFACE ( 'NONE', #8750, 3.800000000000000266 ) ;
#8494 = ORIENTED_EDGE ( 'NONE', *, *, #17938, .F. ) ;
#8495 = ORIENTED_EDGE ( 'NONE', *, *, #4360, .F. ) ;
#8496 = DIRECTION ( 'NONE',  ( 0.000000000000000000, 0.000000000000000000, -1.000000000000000000 ) ) ;
#8497 = APPLICATION_PROTOCOL_DEFINITION ( 'draft international standard', 'automotive_design', 1998, #11393 ) ;
#8498 = ORIENTED_EDGE ( 'NONE', *, *, #16881, .T. ) ;
#8499 = EDGE_CURVE ( 'NONE', #3507, #15861, #14358, .T. ) ;
#8500 = CARTESIAN_POINT ( 'NONE',  ( 56.66441430157296821, 56.09948385550240602, 2.141517661632100111 ) ) ;
#8501 = CARTESIAN_POINT ( 'NONE',  ( 4.175813232069147674, 2.061359961916367833, 3.570380186727398097 ) ) ;
#8502 = AXIS2_PLACEMENT_3D ( 'NONE', #3781, #6421, #15348 ) ;
#8503 = ORIENTED_EDGE ( 'NONE', *, *, #18760, .F. ) ;
#8504 = CIRCLE ( 'NONE', #6010, 12.49999999999999645 ) ;
#8505 = ORIENTED_EDGE ( 'NONE', *, *, #13232, .F. ) ;
#8506 = CYLINDRICAL_SURFACE ( 'NONE', #9887, 15.00000000000000000 ) ;
#8507 = PRODUCT_DEFINITION_SHAPE ( 'NONE', 'NONE',  #13215 ) ;
#8508 = EDGE_CURVE ( 'NONE', #8366, #6538, #3365, .T. ) ;
#8509 = CIRCLE ( 'NONE', #10386, 4.000000000000000000 ) ;
#8510 = VERTEX_POINT ( 'NONE', #2325 ) ;
#8511 = DIRECTION ( 'NONE',  ( -0.000000000000000000, -0.000000000000000000, 1.000000000000000000 ) ) ;
#8512 = ORIENTED_EDGE ( 'NONE', *, *, #1028, .F. ) ;
#8513 = CARTESIAN_POINT ( 'NONE',  ( 50.02271294988512551, 52.49948385550240459, 7.000000000000000888 ) ) ;
#8514 = DIRECTION ( 'NONE',  ( 0.000000000000000000, 0.000000000000000000, -1.000000000000000000 ) ) ;
#8515 = CARTESIAN_POINT ( 'NONE',  ( 50.02271294988505446, 50.50051614449765935, -7.000000000000000888 ) ) ;
#8516 = CARTESIAN_POINT ( 'NONE',  ( 22.14999999999999858, -20.00000000000000000, -23.00000000000000000 ) ) ;
#8517 = DIRECTION ( 'NONE',  ( 0.1305261922200521840, -0.9914448613738103822, 0.000000000000000000 ) ) ;
#8518 = LINE ( 'NONE', #14489, #1899 ) ;
#8519 = PRODUCT_DEFINITION_SHAPE ( 'NONE', 'NONE',  #19420 ) ;
#8520 = CONICAL_SURFACE ( 'NONE', #16987, 5.000000000000000000, 1.047197551196600296 ) ;
#8521 = ORIENTED_EDGE ( 'NONE', *, *, #1375, .F. ) ;
#8522 = ORIENTED_EDGE ( 'NONE', *, *, #11972, .T. ) ;
#8523 = LINE ( 'NONE', #14492, #13099 ) ;
#8524 = CARTESIAN_POINT ( 'NONE',  ( 4.872650870659752442, 0.4273491293402468805, -0.8000000000000000444 ) ) ;
#8525 = ORIENTED_EDGE ( 'NONE', *, *, #2604, .T. ) ;
#8526 = CARTESIAN_POINT ( 'NONE',  ( 6.390820841722129941, 2.823237767533145703, 5.110008744785254464 ) ) ;
#8527 = VERTEX_POINT ( 'NONE', #14064 ) ;
#8528 = ORIENTED_EDGE ( 'NONE', *, *, #9882, .F. ) ;
#8529 = FACE_OUTER_BOUND ( 'NONE', #8551, .T. ) ;
#8530 = CARTESIAN_POINT ( 'NONE',  ( 4.124214193018070240, 4.056676826581888662, 1.068854115921270076E-15 ) ) ;
#8531 = CARTESIAN_POINT ( 'NONE',  ( 44.30067958973594955, 46.10051614449766078, -1.875703265242155693 ) ) ;
#8532 = DIRECTION ( 'NONE',  ( 0.8571673013836855759, 1.049727191973305147E-16, -0.5150380737757258576 ) ) ;
#8533 = CARTESIAN_POINT ( 'NONE',  ( -155.0676494111543491, -18.79939778875158396, -15.79999999999999893 ) ) ;
#8534 = CARTESIAN_POINT ( 'NONE',  ( 49.97728705011488870, 53.49948385550240459, -6.000000000000000888 ) ) ;
#8535 = DIRECTION ( 'NONE',  ( 1.000000000000000000, 0.000000000000000000, 0.000000000000000000 ) ) ;
#8536 = CARTESIAN_POINT ( 'NONE',  ( 43.33558569842703179, 47.09948385550240602, -2.141517661632099223 ) ) ;
#8537 = CARTESIAN_POINT ( 'NONE',  ( 47.37792948025170858, 47.60051614449766078, 7.992620115222797139 ) ) ;
#8538 = DIRECTION ( 'NONE',  ( 0.000000000000000000, -0.000000000000000000, -1.000000000000000000 ) ) ;
#8539 = DIRECTION ( 'NONE',  ( -0.000000000000000000, -0.000000000000000000, -1.000000000000000000 ) ) ;
#8540 = ADVANCED_FACE ( 'NONE', ( #2032 ), #18609, .T. ) ;
#8541 = CARTESIAN_POINT ( 'NONE',  ( 0.000000000000000000, 0.000000000000000000, 0.000000000000000000 ) ) ;
#8542 = VERTEX_POINT ( 'NONE', #17128 ) ;
#8543 = CARTESIAN_POINT ( 'NONE',  ( 30.00000000000000000, 3.000000000000002665, 5.999999999999998224 ) ) ;
#8544 = DIRECTION ( 'NONE',  ( -0.000000000000000000, -0.000000000000000000, 1.000000000000000000 ) ) ;
#8545 = B_SPLINE_CURVE_WITH_KNOTS ( 'NONE', 3,
 ( #5555, #7226, #14569, #3998, #11529, #19017, #17537, #4285 ),
 .UNSPECIFIED., .F., .F.,
 ( 4, 2, 2, 4 ),
 ( 0.002921158011986707288, 0.003648658599403064012, 0.004376159186819420302, 0.005831160361652131148 ),
 .UNSPECIFIED. ) ;
#8546 = CARTESIAN_POINT ( 'NONE',  ( 43.34962307344078880, 56.10051614449766078, -2.184720259617096705 ) ) ;
#8547 = ADVANCED_FACE ( 'NONE', ( #5058 ), #14159, .F. ) ;
#8548 = ADVANCED_FACE ( 'NONE', ( #16936 ), #6815, .T. ) ;
#8549 = CARTESIAN_POINT ( 'NONE',  ( 2.449293598294706513E-15, -20.00000000000000000, 9.000000000000000000 ) ) ;
#8550 = CARTESIAN_POINT ( 'NONE',  ( 54.89903213687075834, 44.74560054925188268, -5.000000000000007105 ) ) ;
#8551 = EDGE_LOOP ( 'NONE', ( #8299, #10752, #7727, #16318 ) ) ;
#8552 = CYLINDRICAL_SURFACE ( 'NONE', #9824, 1.000000000000000888 ) ;
#8553 = EDGE_CURVE ( 'NONE', #7688, #11251, #6716, .T. ) ;
#8554 = DIRECTION ( 'NONE',  ( -0.000000000000000000, -0.000000000000000000, 1.000000000000000000 ) ) ;
#8555 = CARTESIAN_POINT ( 'NONE',  ( 49.97728705011488159, 49.49948385550240459, -7.000000000000000888 ) ) ;
#8556 = EDGE_CURVE ( 'NONE', #5162, #5728, #11219, .T. ) ;
#8557 =( BOUNDED_SURFACE ( )  B_SPLINE_SURFACE ( 3, 2, ( 
 ( #11048, #10954, #16963, #3610, #12528, #11141, #12721, #764, #17148, #13983, #15569, #3518, #9672, #18538, #6735, #15671, #9481, #5270, #570, #17056, #2147, #8109, #2257, #5081, #8213, #18724, #11242, #17250, #15772, #2352, #7134, #5561, #6835, #4101, #2833, #16162, #14483, #7031, #5761, #13013, #17443, #8601, #11439, #4001, #1061, #17733, #5662, #14671, #19019, #17541, #9869, #11727, #2740, #8400, #10069, #13112, #2649, #19119, #8797, #12824, #11532, #16067, #14572, #9961, #4288, #1156, #11635, #3908, #17644, #4194, #8513, #10161, #12917, #15965, #11342, #7230, #5371, #8698, #18827, #10256, #1258, #17349, #14769, #15864, #2446, #14381, #966, #2552, #13208, #16257, #6938, #18921, #19221, #5462, #3021, #18228, #10357, #19318, #13505, #1652, #1350, #16550, #15073, #169, #7425, #11927, #7615, #9182, #13593, #3219, #80, #16360, #9265, #7326, #12216, #6144, #4779, #12116, #4687, #15163, #16742, #261, #18124, #10645, #13301, #5858, #3308, #16653, #6057, #1742, #12023, #14967, #4391, #7705, #1448, #2926, #17830, #7520, #10741, #13684, #6241, #11827, #8888, #14869, #3123, #13401, #17335, #9080, #5960, #17933, #4493, #10449, #16453, #8984, #1546, #18024, #4585, #10543, #18414, #6714, #18509, #12311, #15644, #6621, #15448, #15543, #454, #13780, #17126, #9552, #7989, #9359, #3684, #12598, #18607, #6426, #5056, #9649, #7801, #11217, #10833, #17223, #14157, #4955, #1833, #2122, #370, #2228, #2029, #548, #8188, #3591, #8084, #16934, #5147, #3499, #6519, #740, #3786, #12697, #10928 ),
 ( #14061, #6339, #17033, #16838, #9462, #3398, #18700, #15353, #5245, #12405, #13961, #15253, #11027, #18316, #4872, #11120, #12497, #645, #1937, #7901, #13872, #4077, #2527, #3881, #11610, #7102, #1131, #14356, #18993, #4170, #12799, #8670, #5634, #11320, #12985, #10043, #5532, #16041, #11700, #15745, #8482, #3976, #17516, #939, #14642, #11507, #15939, #6813, #8578, #13085, #11413, #14461, #15839, #18899, #14255, #10135, #8276, #2625, #9751, #1228, #1042, #838, #5738, #18799, #17708, #2322, #9839, #6909, #19093, #7201, #5348, #17324, #12897, #13184, #17417, #19199, #2424, #8376, #7005, #14546, #5435, #17620, #16138, #2716, #9940, #14845, #4561, #12093, #16524, #6122, #16428, #13277, #12190, #10230, #15135, #9055, #1713, #3098, #13373, #16231, #10520, #2805, #18098, #10426, #8958, #4660, #11997, #18000, #5934, #7588, #11895, #14941, #9156, #235, #10618, #7398, #2905, #15043, #7303, #6217, #1625, #7680, #8766, #13569, #19395, #3194, #13661, #1425, #17905, #141, #4264, #16625, #14744, #1330, #19293, #13476, #51, #7494, #4465, #5832, #11801, #2997, #17805, #4361, #1521, #6033, #10326, #16331, #8866, #12471, #1909, #15421, #341, #15519, #18386, #616, #17009, #15329, #11363, #7877, #3474, #7964, #16910, #2002, #10902, #6490, #10718, #9437, #13936, #518, #15889, #18482, #5031, #18200, #11004, #14403, #8055, #6399, #4931, #17371, #3561, #9337, #9528, #3372, #13850, #12377, #9890, #2096, #6593, #14032, #12576, #7780, #18584, #16715, #2473, #431, #13756, #15229, #5392, #3931, #8425 ),
 ( #991, #18290, #1809, #6959, #4757, #3276, #6316, #12289, #9239, #4843, #10805, #16809, #5883, #7348, #5486, #8913, #8531, #14894, #11850, #17856, #4417, #10092, #2670, #13230, #2949, #2858, #17755, #11747, #7257, #2761, #8721, #16181, #16087, #4313, #14501, #11657, #7054, #1085, #4214, #7157, #19240, #13322, #14796, #5785, #8622, #10180, #13037, #10282, #13136, #1373, #16285, #14595, #10382, #1183, #17660, #14695, #1283, #8821, #5689, #19341, #11457, #16385, #1469, #12938, #18946, #17467, #4027, #9988, #15985, #2577, #19043, #19145, #5587, #11557, #17568, #4123, #9200, #12052, #18050, #1675, #18345, #6265, #15283, #7637, #18150, #16477, #4805, #5, #4895, #3147, #3047, #4516, #10672, #13619, #4609, #10571, #290, #16575, #9111, #6081, #12335, #10858, #7544, #10476, #18249, #9388, #5988, #14993, #1574, #13429, #15098, #13529, #391, #6359, #1864, #11954, #3429, #9008, #15379, #16865, #196, #17959, #13713, #103, #9293, #6173, #12143, #7828, #15187, #1764, #4710, #10766, #16676, #3242, #7448, #7734, #13809, #12244, #16767, #3331, #4984, #17351, #767, #6837, #478, #6737, #5085, #18630, #3910, #11244, #9577, #2149, #863, #8111, #12531, #3711, #6547, #18542, #15571, #12826, #12724, #9780, #14088, #12627, #10958, #18726, #13893, #18830, #17059, #16966, #18436, #5171, #676, #11051, #3612, #14185, #6649, #11143, #572, #5373, #11345, #2052, #3520, #5272, #9871, #6448, #9484, #15469, #7922, #17150, #8015, #14281, #1960, #15774, #12429, #13986, #9674, #15673, #2259, #8216, #17253 ),
 ( #3814, #2354, #8304, #5464, #12920, #2651, #19321, #5763, #8701, #6940, #1260, #17832, #11637, #15868, #5861, #4196, #10163, #968, #17646, #11441, #19022, #4004, #11829, #17446, #4394, #1063, #5563, #7328, #19122, #18923, #16260, #7233, #16069, #16164, #7033, #14383, #17735, #2743, #8603, #9963, #4291, #13210, #19223, #13016, #5665, #10258, #15967, #14772, #11729, #2555, #14673, #2835, #8800, #1352, #2448, #8402, #14575, #10071, #13303, #11536, #8515, #14485, #1160, #17543, #4104, #7136, #13114, #9085, #13596, #16553, #1549, #7523, #3221, #14969, #13508, #8986, #15257, #1836, #10451, #13403, #1745, #12314, #2929, #17936, #4496, #16362, #18027, #16456, #3312, #9268, #4782, #8890, #6341, #5963, #18319, #7804, #84, #14871, #16656, #1451, #12221, #3126, #15076, #18231, #18127, #4690, #12026, #13688, #4588, #1655, #13785, #10360, #16745, #6060, #10547, #7708, #12302, #7428, #9184, #373, #11931, #15167, #7619, #3025, #172, #6147, #12119, #10649, #264, #6243, #10744, #3688, #18610, #14065, #650, #8088, #2033, #15647, #6429, #3594, #18418, #12408, #15546, #18514, #5150, #5249, #6717, #11123, #7992, #2126, #4958, #2234, #5059, #12700, #9652, #13964, #17226, #552, #9555, #6625, #12601, #17129, #17036, #8191, #16841, #14160, #743, #18703, #2326, #11220, #3791, #4875, #9756, #841, #15748, #12500, #11030, #8279, #14258, #15451, #6817, #9465, #6523, #12803, #10838, #3402, #9362, #15358, #1942, #13875, #7903, #456, #10931, #16939, #3503, #15842, #11704, #2531, #4080, #8581, #17520 ),
 ( #2427, #17624, #16142, #1045, #10048, #5440, #8489, #3885, #19202, #17328, #7105, #18802, #17711, #16046, #9842, #14749, #8379, #1333, #5353, #12901, #3979, #2719, #10233, #14360, #943, #9943, #4268, #7009, #16235, #6915, #18902, #11510, #19097, #11324, #14549, #13088, #4174, #11416, #15942, #5637, #7204, #11614, #1232, #2628, #17420, #7306, #14465, #2809, #10139, #8770, #8675, #14645, #13189, #12989, #18996, #5741, #5535, #1135, #1812, #9243, #3198, #6036, #4663, #12000, #7498, #16336, #7591, #13376, #2908, #10329, #56, #16719, #9159, #6125, #4366, #18101, #15232, #9057, #13281, #3279, #1629, #13571, #17809, #15047, #8869, #16432, #1428, #19297, #14849, #5835, #17909, #3000, #4761, #16528, #7402, #13664, #10622, #13478, #144, #4468, #11805, #15138, #12096, #18004, #19399, #1716, #16628, #7683, #10429, #3101, #239, #5936, #12194, #6220, #11898, #18203, #8961, #14944, #1524, #10721, #4564, #10523, #4935, #621, #12380, #10906, #6402, #12676, #18678, #7880, #10807, #18589, #9725, #345, #15333, #1912, #13759, #15427, #13853, #722, #6692, #2200, #6320, #3758, #3376, #15722, #5221, #16914, #12293, #14036, #18293, #9626, #13940, #12474, #15620, #15523, #2100, #9441, #11097, #2006, #18487, #11195, #7782, #14136, #3477, #18389, #5126, #16813, #4846, #6597, #17201, #9339, #12580, #7968, #433, #521, #6495, #5035, #8060, #11008, #17104, #3663, #8162, #17015, #3566, #9531, #5511, #18876, #13064, #3859, #1020, #15819, #9819, #12962, #15916, #16020, #2694, #4154, #2606, #5415, #18971 ),
 ( #17493, #8559, #4242, #8256, #14439, #2503, #10018, #6886, #1207, #4055, #8458, #18776, #1110, #19072, #3956, #6982, #8353, #11388, #6789, #8648, #817, #14524, #2303, #7182, #11484, #12775, #17688, #5321, #10205, #14232, #2400, #12874, #5614, #13162, #11295, #17302, #17397, #9918, #7081, #19177, #11587, #14331, #14621, #17599, #10118, #16116, #5719, #915, #11685, #10500, #8940, #10307, #18077, #13552, #7570, #1403, #6017, #10600, #19272, #15120, #12075, #17780, #32, #16505, #11979, #3078, #18180, #2785, #14924, #10409, #4541, #7379, #1696, #17983, #2975, #13256, #15022, #125, #17884, #1499, #2887, #5906, #1311, #16603, #14725, #9034, #16208, #7663, #7473, #7280, #12172, #5811, #4739, #8747, #16314, #13352, #6105, #13644, #11777, #4339, #19372, #219, #4448, #6199, #8848, #14823, #13453, #1601, #11875, #4640, #3176, #9136, #16408, #1890, #10987, #18567, #3549, #12560, #3455, #323, #18662, #16699, #2177, #15498, #8141, #9508, #14014, #5109, #6673, #9600, #16994, #2076, #10700, #3263, #12655, #598, #9421, #8038, #15407, #4917, #13737, #5010, #10789, #6299, #7762, #16892, #14116, #6574, #11079, #1792, #17084, #9224, #6475, #15214, #702, #18464, #3640, #12273, #12454, #18272, #13834, #4826, #16792, #3358, #9320, #15309, #15597, #7861, #415, #6380, #1984, #12359, #18369, #10886, #7948, #13916, #503, #997, #5199, #8628, #12943, #18952, #9703, #6964, #798, #8332, #12752, #14601, #6769, #1190, #9801, #14312, #16092, #8432, #2282, #5593, #15994, #5397, #5492, #15797, #3736 ),
 ( #2583, #2378, #14411, #19050, #8236, #4130, #1091, #18749, #11462, #17474, #4033, #9995, #7162, #11169, #17376, #18856, #8536, #890, #10097, #14506, #11369, #14210, #7061, #13042, #6859, #3937, #11269, #12848, #15703, #11562, #5295, #17578, #17177, #2675, #15896, #17280, #13141, #3840, #9895, #2480, #13237, #4320, #16747, #10840, #2768, #8726, #10288, #18321, #1380, #16845, #14700, #17664, #11855, #9, #19153, #14901, #13434, #17964, #5789, #16291, #5997, #7809, #11961, #1838, #17862, #1291, #7906, #5697, #3405, #4522, #9366, #10746, #3314, #13788, #15361, #4877, #9271, #15261, #11663, #4219, #1944, #375, #4425, #6344, #10389, #13327, #12316, #10186, #16186, #8920, #1475, #2955, #2865, #7263, #19247, #16390, #11753, #17760, #7453, #19347, #8828, #14801, #7354, #5889, #18518, #654, #9467, #8195, #9557, #6719, #9654, #12507, #11222, #5060, #8090, #12603, #14067, #6627, #15547, #5152, #458, #18612, #11126, #17131, #15752, #3690, #2127, #13877, #15652, #6431, #12703, #2237, #14163, #2330, #745, #11031, #18706, #17037, #3595, #5251, #8282, #17229, #3795, #9758, #14261, #15453, #844, #4962, #12410, #18420, #554, #2035, #10936, #16942, #3505, #7994, #13966, #6525, #9149, #10613, #16905, #3468, #12088, #15037, #3367, #13931, #4554, #136, #6117, #17994, #230, #18092, #4926, #10895, #6394, #10513, #7959, #7581, #511, #9431, #1708, #16518, #18284, #3091, #13844, #18194, #16709, #426, #334, #6311, #13656, #15324, #6209, #3270, #15415, #11991, #18379, #15129, #16619, #9331, #1619 ) ),
 .UNSPECIFIED., .T., .F., .T. ) 
 B_SPLINE_SURFACE_WITH_KNOTS ( ( 4, 3, 4 ),
 ( 3, 2, 2, 2, 2, 2, 2, 2, 2, 2, 2, 2, 2, 2, 2, 2, 2, 2, 2, 2, 2, 2, 2, 2, 2, 2, 2, 2, 2, 2, 2, 2, 2, 2, 2, 2, 2, 2, 2, 2, 2, 2, 2, 2, 2, 2, 2, 2, 2, 2, 2, 2, 2, 2, 2, 2, 2, 2, 2, 2, 2, 2, 2, 2, 2, 2, 2, 2, 2, 2, 2, 2, 2, 2, 2, 2, 2, 2, 2, 2, 2, 2, 2, 2, 2, 2, 2, 2, 2, 2, 2, 2, 2, 2, 2, 2, 2, 2, 2, 2, 3 ),
 ( 0.000000000000000000, 0.5000000000000000000, 1.000000000000000000 ),
 ( 0.000000000000000000, 0.01000000000000000021, 0.02000000000000000042, 0.02999999999999999889, 0.04000000000000000083, 0.05000000000000000278, 0.05999999999999999778, 0.07000000000000000666, 0.08000000000000000167, 0.08999999999999999667, 0.1000000000000000056, 0.1100000000000000006, 0.1199999999999999956, 0.1300000000000000044, 0.1400000000000000133, 0.1499999999999999944, 0.1600000000000000033, 0.1700000000000000122, 0.1799999999999999933, 0.1900000000000000022, 0.2000000000000000111, 0.2099999999999999922, 0.2200000000000000011, 0.2300000000000000100, 0.2399999999999999911, 0.2500000000000000000, 0.2600000000000000089, 0.2700000000000000178, 0.2800000000000000266, 0.2899999999999999800, 0.2999999999999999889, 0.3099999999999999978, 0.3200000000000000067, 0.3300000000000000155, 0.3400000000000000244, 0.3499999999999999778, 0.3599999999999999867, 0.3699999999999999956, 0.3800000000000000044, 0.3900000000000000133, 0.4000000000000000222, 0.4099999999999999756, 0.4199999999999999845, 0.4299999999999999933, 0.4400000000000000022, 0.4500000000000000111, 0.4600000000000000200, 0.4699999999999999734, 0.4799999999999999822, 0.4899999999999999911, 0.5000000000000000000, 0.5100000000000000089, 0.5200000000000000178, 0.5300000000000000266, 0.5400000000000000355, 0.5500000000000000444, 0.5600000000000000533, 0.5699999999999999512, 0.5799999999999999600, 0.5899999999999999689, 0.5999999999999999778, 0.6099999999999999867, 0.6199999999999999956, 0.6300000000000000044, 0.6400000000000000133, 0.6500000000000000222, 0.6600000000000000311, 0.6700000000000000400, 0.6800000000000000488, 0.6899999999999999467, 0.6999999999999999556, 0.7099999999999999645, 0.7199999999999999734, 0.7299999999999999822, 0.7399999999999999911, 0.7500000000000000000, 0.7600000000000000089, 0.7700000000000000178, 0.7800000000000000266, 0.7900000000000000355, 0.8000000000000000444, 0.8100000000000000533, 0.8199999999999999512, 0.8299999999999999600, 0.8399999999999999689, 0.8499999999999999778, 0.8599999999999999867, 0.8699999999999999956, 0.8800000000000000044, 0.8900000000000000133, 0.9000000000000000222, 0.9100000000000000311, 0.9200000000000000400, 0.9300000000000000488, 0.9399999999999999467, 0.9499999999999999556, 0.9599999999999999645, 0.9699999999999999734, 0.9799999999999999822, 0.9899999999999999911, 1.000000000000000000 ),
 .UNSPECIFIED. ) 
 GEOMETRIC_REPRESENTATION_ITEM ( )  RATIONAL_B_SPLINE_SURFACE ( (
 ( 1.000000000000000000, 0.9510565162951535312, 1.000000000000000000, 0.9510565162951535312, 1.000000000000000000, 0.9510565162951535312, 1.000000000000000000, 0.9510565162951535312, 1.000000000000000000, 0.9510565162951535312, 1.000000000000000000, 0.9510565162951535312, 1.000000000000000000, 0.9510565162951535312, 1.000000000000000000, 0.9510565162951535312, 1.000000000000000000, 0.9510565162951535312, 1.000000000000000000, 0.9510565162951535312, 1.000000000000000000, 0.9510565162951535312, 1.000000000000000000, 0.9510565162951535312, 1.000000000000000000, 0.9510565162951535312, 1.000000000000000000, 0.9510565162951535312, 1.000000000000000000, 0.9510565162951535312, 1.000000000000000000, 0.9510565162951535312, 1.000000000000000000, 0.9510565162951535312, 1.000000000000000000, 0.9510565162951535312, 1.000000000000000000, 0.9510565162951535312, 1.000000000000000000, 0.9510565162951535312, 1.000000000000000000, 0.9510565162951535312, 1.000000000000000000, 0.9510565162951535312, 1.000000000000000000, 0.9510565162951535312, 1.000000000000000000, 0.9510565162951535312, 1.000000000000000000, 0.9510565162951535312, 1.000000000000000000, 0.9510565162951535312, 1.000000000000000000, 0.9510565162951535312, 1.000000000000000000, 0.9510565162951535312, 1.000000000000000000, 0.9510565162951535312, 1.000000000000000000, 0.9510565162951535312, 1.000000000000000000, 0.9510565162951535312, 1.000000000000000000, 0.9510565162951535312, 1.000000000000000000, 0.9510565162951535312, 1.000000000000000000, 0.9510565162951535312, 1.000000000000000000, 0.9510565162951535312, 1.000000000000000000, 0.9510565162951535312, 1.000000000000000000, 0.9510565162951535312, 1.000000000000000000, 0.9510565162951535312, 1.000000000000000000, 0.9510565162951535312, 1.000000000000000000, 0.9510565162951535312, 1.000000000000000000, 0.9510565162951535312, 1.000000000000000000, 0.9510565162951535312, 1.000000000000000000, 0.9510565162951535312, 1.000000000000000000, 0.9510565162951535312, 1.000000000000000000, 0.9510565162951535312, 1.000000000000000000, 0.9510565162951535312, 1.000000000000000000, 0.9510565162951535312, 1.000000000000000000, 0.9510565162951535312, 1.000000000000000000, 0.9510565162951535312, 1.000000000000000000, 0.9510565162951535312, 1.000000000000000000, 0.9510565162951535312, 1.000000000000000000, 0.9510565162951535312, 1.000000000000000000, 0.9510565162951535312, 1.000000000000000000, 0.9510565162951535312, 1.000000000000000000, 0.9510565162951535312, 1.000000000000000000, 0.9510565162951535312, 1.000000000000000000, 0.9510565162951535312, 1.000000000000000000, 0.9510565162951535312, 1.000000000000000000, 0.9510565162951535312, 1.000000000000000000, 0.9510565162951535312, 1.000000000000000000, 0.9510565162951535312, 1.000000000000000000, 0.9510565162951535312, 1.000000000000000000, 0.9510565162951535312, 1.000000000000000000, 0.9510565162951535312, 1.000000000000000000, 0.9510565162951535312, 1.000000000000000000, 0.9510565162951535312, 1.000000000000000000, 0.9510565162951535312, 1.000000000000000000, 0.9510565162951535312, 1.000000000000000000, 0.9510565162951535312, 1.000000000000000000, 0.9510565162951535312, 1.000000000000000000, 0.9510565162951535312, 1.000000000000000000, 0.9510565162951535312, 1.000000000000000000, 0.9510565162951535312, 1.000000000000000000, 0.9510565162951535312, 1.000000000000000000, 0.9510565162951535312, 1.000000000000000000, 0.9510565162951535312, 1.000000000000000000, 0.9510565162951535312, 1.000000000000000000, 0.9510565162951535312, 1.000000000000000000, 0.9510565162951535312, 1.000000000000000000, 0.9510565162951535312, 1.000000000000000000, 0.9510565162951535312, 1.000000000000000000, 0.9510565162951535312, 1.000000000000000000, 0.9510565162951535312, 1.000000000000000000, 0.9510565162951535312, 1.000000000000000000, 0.9510565162951535312, 1.000000000000000000, 0.9510565162951535312, 1.000000000000000000, 0.9510565162951535312, 1.000000000000000000, 0.9510565162951535312, 1.000000000000000000, 0.9510565162951535312, 1.000000000000000000, 0.9510565162951535312, 1.000000000000000000, 0.9510565162951535312, 1.000000000000000000, 0.9510565162951535312, 1.000000000000000000, 0.9510565162951535312, 1.000000000000000000, 0.9510565162951535312, 1.000000000000000000, 0.9510565162951535312, 1.000000000000000000, 0.9510565162951535312, 1.000000000000000000, 0.9510565162951535312, 1.000000000000000000, 0.9510565162951535312, 1.000000000000000000, 0.9510565162951535312, 1.000000000000000000, 0.9510565162951535312, 1.000000000000000000),
 ( 0.3333333333333333703, 0.3170188387650512141, 0.3333333333333333703, 0.3170188387650512141, 0.3333333333333333703, 0.3170188387650512141, 0.3333333333333333703, 0.3170188387650512141, 0.3333333333333333703, 0.3170188387650512141, 0.3333333333333333703, 0.3170188387650512141, 0.3333333333333333703, 0.3170188387650512141, 0.3333333333333333703, 0.3170188387650512141, 0.3333333333333333703, 0.3170188387650512141, 0.3333333333333333703, 0.3170188387650512141, 0.3333333333333333703, 0.3170188387650512141, 0.3333333333333333703, 0.3170188387650512141, 0.3333333333333333703, 0.3170188387650512141, 0.3333333333333333703, 0.3170188387650512141, 0.3333333333333333703, 0.3170188387650512141, 0.3333333333333333703, 0.3170188387650512141, 0.3333333333333333703, 0.3170188387650512141, 0.3333333333333333703, 0.3170188387650512141, 0.3333333333333333703, 0.3170188387650512141, 0.3333333333333333703, 0.3170188387650512141, 0.3333333333333333703, 0.3170188387650512141, 0.3333333333333333703, 0.3170188387650512141, 0.3333333333333333703, 0.3170188387650512141, 0.3333333333333333703, 0.3170188387650512141, 0.3333333333333333703, 0.3170188387650512141, 0.3333333333333333703, 0.3170188387650512141, 0.3333333333333333703, 0.3170188387650512141, 0.3333333333333333703, 0.3170188387650512141, 0.3333333333333333703, 0.3170188387650512141, 0.3333333333333333703, 0.3170188387650512141, 0.3333333333333333703, 0.3170188387650512141, 0.3333333333333333703, 0.3170188387650512141, 0.3333333333333333703, 0.3170188387650512141, 0.3333333333333333703, 0.3170188387650512141, 0.3333333333333333703, 0.3170188387650512141, 0.3333333333333333703, 0.3170188387650512141, 0.3333333333333333703, 0.3170188387650512141, 0.3333333333333333703, 0.3170188387650512141, 0.3333333333333333703, 0.3170188387650512141, 0.3333333333333333703, 0.3170188387650512141, 0.3333333333333333703, 0.3170188387650512141, 0.3333333333333333703, 0.3170188387650512141, 0.3333333333333333703, 0.3170188387650512141, 0.3333333333333333703, 0.3170188387650512141, 0.3333333333333333703, 0.3170188387650512141, 0.3333333333333333703, 0.3170188387650512141, 0.3333333333333333703, 0.3170188387650512141, 0.3333333333333333703, 0.3170188387650512141, 0.3333333333333333703, 0.3170188387650512141, 0.3333333333333333703, 0.3170188387650512141, 0.3333333333333333703, 0.3170188387650512141, 0.3333333333333333703, 0.3170188387650512141, 0.3333333333333333703, 0.3170188387650512141, 0.3333333333333333703, 0.3170188387650512141, 0.3333333333333333703, 0.3170188387650512141, 0.3333333333333333703, 0.3170188387650512141, 0.3333333333333333703, 0.3170188387650512141, 0.3333333333333333703, 0.3170188387650512141, 0.3333333333333333703, 0.3170188387650512141, 0.3333333333333333703, 0.3170188387650512141, 0.3333333333333333703, 0.3170188387650512141, 0.3333333333333333703, 0.3170188387650512141, 0.3333333333333333703, 0.3170188387650512141, 0.3333333333333333703, 0.3170188387650512141, 0.3333333333333333703, 0.3170188387650512141, 0.3333333333333333703, 0.3170188387650512141, 0.3333333333333333703, 0.3170188387650512141, 0.3333333333333333703, 0.3170188387650512141, 0.3333333333333333703, 0.3170188387650512141, 0.3333333333333333703, 0.3170188387650512141, 0.3333333333333333703, 0.3170188387650512141, 0.3333333333333333703, 0.3170188387650512141, 0.3333333333333333703, 0.3170188387650512141, 0.3333333333333333703, 0.3170188387650512141, 0.3333333333333333703, 0.3170188387650512141, 0.3333333333333333703, 0.3170188387650512141, 0.3333333333333333703, 0.3170188387650512141, 0.3333333333333333703, 0.3170188387650512141, 0.3333333333333333703, 0.3170188387650512141, 0.3333333333333333703, 0.3170188387650512141, 0.3333333333333333703, 0.3170188387650512141, 0.3333333333333333703, 0.3170188387650512141, 0.3333333333333333703, 0.3170188387650512141, 0.3333333333333333703, 0.3170188387650512141, 0.3333333333333333703, 0.3170188387650512141, 0.3333333333333333703, 0.3170188387650512141, 0.3333333333333333703, 0.3170188387650512141, 0.3333333333333333703, 0.3170188387650512141, 0.3333333333333333703, 0.3170188387650512141, 0.3333333333333333703, 0.3170188387650512141, 0.3333333333333333703, 0.3170188387650512141, 0.3333333333333333703, 0.3170188387650512141, 0.3333333333333333703, 0.3170188387650512141, 0.3333333333333333703, 0.3170188387650512141, 0.3333333333333333703, 0.3170188387650512141, 0.3333333333333333703, 0.3170188387650512141, 0.3333333333333333703, 0.3170188387650512141, 0.3333333333333333703, 0.3170188387650512141, 0.3333333333333333703, 0.3170188387650512141, 0.3333333333333333703, 0.3170188387650512141, 0.3333333333333333703),
 ( 0.3333333333333333703, 0.3170188387650512141, 0.3333333333333333703, 0.3170188387650512141, 0.3333333333333333703, 0.3170188387650512141, 0.3333333333333333703, 0.3170188387650512141, 0.3333333333333333703, 0.3170188387650512141, 0.3333333333333333703, 0.3170188387650512141, 0.3333333333333333703, 0.3170188387650512141, 0.3333333333333333703, 0.3170188387650512141, 0.3333333333333333703, 0.3170188387650512141, 0.3333333333333333703, 0.3170188387650512141, 0.3333333333333333703, 0.3170188387650512141, 0.3333333333333333703, 0.3170188387650512141, 0.3333333333333333703, 0.3170188387650512141, 0.3333333333333333703, 0.3170188387650512141, 0.3333333333333333703, 0.3170188387650512141, 0.3333333333333333703, 0.3170188387650512141, 0.3333333333333333703, 0.3170188387650512141, 0.3333333333333333703, 0.3170188387650512141, 0.3333333333333333703, 0.3170188387650512141, 0.3333333333333333703, 0.3170188387650512141, 0.3333333333333333703, 0.3170188387650512141, 0.3333333333333333703, 0.3170188387650512141, 0.3333333333333333703, 0.3170188387650512141, 0.3333333333333333703, 0.3170188387650512141, 0.3333333333333333703, 0.3170188387650512141, 0.3333333333333333703, 0.3170188387650512141, 0.3333333333333333703, 0.3170188387650512141, 0.3333333333333333703, 0.3170188387650512141, 0.3333333333333333703, 0.3170188387650512141, 0.3333333333333333703, 0.3170188387650512141, 0.3333333333333333703, 0.3170188387650512141, 0.3333333333333333703, 0.3170188387650512141, 0.3333333333333333703, 0.3170188387650512141, 0.3333333333333333703, 0.3170188387650512141, 0.3333333333333333703, 0.3170188387650512141, 0.3333333333333333703, 0.3170188387650512141, 0.3333333333333333703, 0.3170188387650512141, 0.3333333333333333703, 0.3170188387650512141, 0.3333333333333333703, 0.3170188387650512141, 0.3333333333333333703, 0.3170188387650512141, 0.3333333333333333703, 0.3170188387650512141, 0.3333333333333333703, 0.3170188387650512141, 0.3333333333333333703, 0.3170188387650512141, 0.3333333333333333703, 0.3170188387650512141, 0.3333333333333333703, 0.3170188387650512141, 0.3333333333333333703, 0.3170188387650512141, 0.3333333333333333703, 0.3170188387650512141, 0.3333333333333333703, 0.3170188387650512141, 0.3333333333333333703, 0.3170188387650512141, 0.3333333333333333703, 0.3170188387650512141, 0.3333333333333333703, 0.3170188387650512141, 0.3333333333333333703, 0.3170188387650512141, 0.3333333333333333703, 0.3170188387650512141, 0.3333333333333333703, 0.3170188387650512141, 0.3333333333333333703, 0.3170188387650512141, 0.3333333333333333703, 0.3170188387650512141, 0.3333333333333333703, 0.3170188387650512141, 0.3333333333333333703, 0.3170188387650512141, 0.3333333333333333703, 0.3170188387650512141, 0.3333333333333333703, 0.3170188387650512141, 0.3333333333333333703, 0.3170188387650512141, 0.3333333333333333703, 0.3170188387650512141, 0.3333333333333333703, 0.3170188387650512141, 0.3333333333333333703, 0.3170188387650512141, 0.3333333333333333703, 0.3170188387650512141, 0.3333333333333333703, 0.3170188387650512141, 0.3333333333333333703, 0.3170188387650512141, 0.3333333333333333703, 0.3170188387650512141, 0.3333333333333333703, 0.3170188387650512141, 0.3333333333333333703, 0.3170188387650512141, 0.3333333333333333703, 0.3170188387650512141, 0.3333333333333333703, 0.3170188387650512141, 0.3333333333333333703, 0.3170188387650512141, 0.3333333333333333703, 0.3170188387650512141, 0.3333333333333333703, 0.3170188387650512141, 0.3333333333333333703, 0.3170188387650512141, 0.3333333333333333703, 0.3170188387650512141, 0.3333333333333333703, 0.3170188387650512141, 0.3333333333333333703, 0.3170188387650512141, 0.3333333333333333703, 0.3170188387650512141, 0.3333333333333333703, 0.3170188387650512141, 0.3333333333333333703, 0.3170188387650512141, 0.3333333333333333703, 0.3170188387650512141, 0.3333333333333333703, 0.3170188387650512141, 0.3333333333333333703, 0.3170188387650512141, 0.3333333333333333703, 0.3170188387650512141, 0.3333333333333333703, 0.3170188387650512141, 0.3333333333333333703, 0.3170188387650512141, 0.3333333333333333703, 0.3170188387650512141, 0.3333333333333333703, 0.3170188387650512141, 0.3333333333333333703, 0.3170188387650512141, 0.3333333333333333703, 0.3170188387650512141, 0.3333333333333333703, 0.3170188387650512141, 0.3333333333333333703, 0.3170188387650512141, 0.3333333333333333703, 0.3170188387650512141, 0.3333333333333333703, 0.3170188387650512141, 0.3333333333333333703, 0.3170188387650512141, 0.3333333333333333703, 0.3170188387650512141, 0.3333333333333333703, 0.3170188387650512141, 0.3333333333333333703, 0.3170188387650512141, 0.3333333333333333703),
 ( 1.000000000000000000, 0.9510565162951535312, 1.000000000000000000, 0.9510565162951535312, 1.000000000000000000, 0.9510565162951535312, 1.000000000000000000, 0.9510565162951535312, 1.000000000000000000, 0.9510565162951535312, 1.000000000000000000, 0.9510565162951535312, 1.000000000000000000, 0.9510565162951535312, 1.000000000000000000, 0.9510565162951535312, 1.000000000000000000, 0.9510565162951535312, 1.000000000000000000, 0.9510565162951535312, 1.000000000000000000, 0.9510565162951535312, 1.000000000000000000, 0.9510565162951535312, 1.000000000000000000, 0.9510565162951535312, 1.000000000000000000, 0.9510565162951535312, 1.000000000000000000, 0.9510565162951535312, 1.000000000000000000, 0.9510565162951535312, 1.000000000000000000, 0.9510565162951535312, 1.000000000000000000, 0.9510565162951535312, 1.000000000000000000, 0.9510565162951535312, 1.000000000000000000, 0.9510565162951535312, 1.000000000000000000, 0.9510565162951535312, 1.000000000000000000, 0.9510565162951535312, 1.000000000000000000, 0.9510565162951535312, 1.000000000000000000, 0.9510565162951535312, 1.000000000000000000, 0.9510565162951535312, 1.000000000000000000, 0.9510565162951535312, 1.000000000000000000, 0.9510565162951535312, 1.000000000000000000, 0.9510565162951535312, 1.000000000000000000, 0.9510565162951535312, 1.000000000000000000, 0.9510565162951535312, 1.000000000000000000, 0.9510565162951535312, 1.000000000000000000, 0.9510565162951535312, 1.000000000000000000, 0.9510565162951535312, 1.000000000000000000, 0.9510565162951535312, 1.000000000000000000, 0.9510565162951535312, 1.000000000000000000, 0.9510565162951535312, 1.000000000000000000, 0.9510565162951535312, 1.000000000000000000, 0.9510565162951535312, 1.000000000000000000, 0.9510565162951535312, 1.000000000000000000, 0.9510565162951535312, 1.000000000000000000, 0.9510565162951535312, 1.000000000000000000, 0.9510565162951535312, 1.000000000000000000, 0.9510565162951535312, 1.000000000000000000, 0.9510565162951535312, 1.000000000000000000, 0.9510565162951535312, 1.000000000000000000, 0.9510565162951535312, 1.000000000000000000, 0.9510565162951535312, 1.000000000000000000, 0.9510565162951535312, 1.000000000000000000, 0.9510565162951535312, 1.000000000000000000, 0.9510565162951535312, 1.000000000000000000, 0.9510565162951535312, 1.000000000000000000, 0.9510565162951535312, 1.000000000000000000, 0.9510565162951535312, 1.000000000000000000, 0.9510565162951535312, 1.000000000000000000, 0.9510565162951535312, 1.000000000000000000, 0.9510565162951535312, 1.000000000000000000, 0.9510565162951535312, 1.000000000000000000, 0.9510565162951535312, 1.000000000000000000, 0.9510565162951535312, 1.000000000000000000, 0.9510565162951535312, 1.000000000000000000, 0.9510565162951535312, 1.000000000000000000, 0.9510565162951535312, 1.000000000000000000, 0.9510565162951535312, 1.000000000000000000, 0.9510565162951535312, 1.000000000000000000, 0.9510565162951535312, 1.000000000000000000, 0.9510565162951535312, 1.000000000000000000, 0.9510565162951535312, 1.000000000000000000, 0.9510565162951535312, 1.000000000000000000, 0.9510565162951535312, 1.000000000000000000, 0.9510565162951535312, 1.000000000000000000, 0.9510565162951535312, 1.000000000000000000, 0.9510565162951535312, 1.000000000000000000, 0.9510565162951535312, 1.000000000000000000, 0.9510565162951535312, 1.000000000000000000, 0.9510565162951535312, 1.000000000000000000, 0.9510565162951535312, 1.000000000000000000, 0.9510565162951535312, 1.000000000000000000, 0.9510565162951535312, 1.000000000000000000, 0.9510565162951535312, 1.000000000000000000, 0.9510565162951535312, 1.000000000000000000, 0.9510565162951535312, 1.000000000000000000, 0.9510565162951535312, 1.000000000000000000, 0.9510565162951535312, 1.000000000000000000, 0.9510565162951535312, 1.000000000000000000, 0.9510565162951535312, 1.000000000000000000, 0.9510565162951535312, 1.000000000000000000, 0.9510565162951535312, 1.000000000000000000, 0.9510565162951535312, 1.000000000000000000, 0.9510565162951535312, 1.000000000000000000, 0.9510565162951535312, 1.000000000000000000, 0.9510565162951535312, 1.000000000000000000, 0.9510565162951535312, 1.000000000000000000, 0.9510565162951535312, 1.000000000000000000, 0.9510565162951535312, 1.000000000000000000, 0.9510565162951535312, 1.000000000000000000, 0.9510565162951535312, 1.000000000000000000, 0.9510565162951535312, 1.000000000000000000, 0.9510565162951535312, 1.000000000000000000, 0.9510565162951535312, 1.000000000000000000, 0.9510565162951535312, 1.000000000000000000),
 ( 0.3333333333333333703, 0.3170188387650512141, 0.3333333333333333703, 0.3170188387650512141, 0.3333333333333333703, 0.3170188387650512141, 0.3333333333333333703, 0.3170188387650512141, 0.3333333333333333703, 0.3170188387650512141, 0.3333333333333333703, 0.3170188387650512141, 0.3333333333333333703, 0.3170188387650512141, 0.3333333333333333703, 0.3170188387650512141, 0.3333333333333333703, 0.3170188387650512141, 0.3333333333333333703, 0.3170188387650512141, 0.3333333333333333703, 0.3170188387650512141, 0.3333333333333333703, 0.3170188387650512141, 0.3333333333333333703, 0.3170188387650512141, 0.3333333333333333703, 0.3170188387650512141, 0.3333333333333333703, 0.3170188387650512141, 0.3333333333333333703, 0.3170188387650512141, 0.3333333333333333703, 0.3170188387650512141, 0.3333333333333333703, 0.3170188387650512141, 0.3333333333333333703, 0.3170188387650512141, 0.3333333333333333703, 0.3170188387650512141, 0.3333333333333333703, 0.3170188387650512141, 0.3333333333333333703, 0.3170188387650512141, 0.3333333333333333703, 0.3170188387650512141, 0.3333333333333333703, 0.3170188387650512141, 0.3333333333333333703, 0.3170188387650512141, 0.3333333333333333703, 0.3170188387650512141, 0.3333333333333333703, 0.3170188387650512141, 0.3333333333333333703, 0.3170188387650512141, 0.3333333333333333703, 0.3170188387650512141, 0.3333333333333333703, 0.3170188387650512141, 0.3333333333333333703, 0.3170188387650512141, 0.3333333333333333703, 0.3170188387650512141, 0.3333333333333333703, 0.3170188387650512141, 0.3333333333333333703, 0.3170188387650512141, 0.3333333333333333703, 0.3170188387650512141, 0.3333333333333333703, 0.3170188387650512141, 0.3333333333333333703, 0.3170188387650512141, 0.3333333333333333703, 0.3170188387650512141, 0.3333333333333333703, 0.3170188387650512141, 0.3333333333333333703, 0.3170188387650512141, 0.3333333333333333703, 0.3170188387650512141, 0.3333333333333333703, 0.3170188387650512141, 0.3333333333333333703, 0.3170188387650512141, 0.3333333333333333703, 0.3170188387650512141, 0.3333333333333333703, 0.3170188387650512141, 0.3333333333333333703, 0.3170188387650512141, 0.3333333333333333703, 0.3170188387650512141, 0.3333333333333333703, 0.3170188387650512141, 0.3333333333333333703, 0.3170188387650512141, 0.3333333333333333703, 0.3170188387650512141, 0.3333333333333333703, 0.3170188387650512141, 0.3333333333333333703, 0.3170188387650512141, 0.3333333333333333703, 0.3170188387650512141, 0.3333333333333333703, 0.3170188387650512141, 0.3333333333333333703, 0.3170188387650512141, 0.3333333333333333703, 0.3170188387650512141, 0.3333333333333333703, 0.3170188387650512141, 0.3333333333333333703, 0.3170188387650512141, 0.3333333333333333703, 0.3170188387650512141, 0.3333333333333333703, 0.3170188387650512141, 0.3333333333333333703, 0.3170188387650512141, 0.3333333333333333703, 0.3170188387650512141, 0.3333333333333333703, 0.3170188387650512141, 0.3333333333333333703, 0.3170188387650512141, 0.3333333333333333703, 0.3170188387650512141, 0.3333333333333333703, 0.3170188387650512141, 0.3333333333333333703, 0.3170188387650512141, 0.3333333333333333703, 0.3170188387650512141, 0.3333333333333333703, 0.3170188387650512141, 0.3333333333333333703, 0.3170188387650512141, 0.3333333333333333703, 0.3170188387650512141, 0.3333333333333333703, 0.3170188387650512141, 0.3333333333333333703, 0.3170188387650512141, 0.3333333333333333703, 0.3170188387650512141, 0.3333333333333333703, 0.3170188387650512141, 0.3333333333333333703, 0.3170188387650512141, 0.3333333333333333703, 0.3170188387650512141, 0.3333333333333333703, 0.3170188387650512141, 0.3333333333333333703, 0.3170188387650512141, 0.3333333333333333703, 0.3170188387650512141, 0.3333333333333333703, 0.3170188387650512141, 0.3333333333333333703, 0.3170188387650512141, 0.3333333333333333703, 0.3170188387650512141, 0.3333333333333333703, 0.3170188387650512141, 0.3333333333333333703, 0.3170188387650512141, 0.3333333333333333703, 0.3170188387650512141, 0.3333333333333333703, 0.3170188387650512141, 0.3333333333333333703, 0.3170188387650512141, 0.3333333333333333703, 0.3170188387650512141, 0.3333333333333333703, 0.3170188387650512141, 0.3333333333333333703, 0.3170188387650512141, 0.3333333333333333703, 0.3170188387650512141, 0.3333333333333333703, 0.3170188387650512141, 0.3333333333333333703, 0.3170188387650512141, 0.3333333333333333703, 0.3170188387650512141, 0.3333333333333333703, 0.3170188387650512141, 0.3333333333333333703, 0.3170188387650512141, 0.3333333333333333703, 0.3170188387650512141, 0.3333333333333333703, 0.3170188387650512141, 0.3333333333333333703, 0.3170188387650512141, 0.3333333333333333703),
 ( 0.3333333333333333703, 0.3170188387650512141, 0.3333333333333333703, 0.3170188387650512141, 0.3333333333333333703, 0.3170188387650512141, 0.3333333333333333703, 0.3170188387650512141, 0.3333333333333333703, 0.3170188387650512141, 0.3333333333333333703, 0.3170188387650512141, 0.3333333333333333703, 0.3170188387650512141, 0.3333333333333333703, 0.3170188387650512141, 0.3333333333333333703, 0.3170188387650512141, 0.3333333333333333703, 0.3170188387650512141, 0.3333333333333333703, 0.3170188387650512141, 0.3333333333333333703, 0.3170188387650512141, 0.3333333333333333703, 0.3170188387650512141, 0.3333333333333333703, 0.3170188387650512141, 0.3333333333333333703, 0.3170188387650512141, 0.3333333333333333703, 0.3170188387650512141, 0.3333333333333333703, 0.3170188387650512141, 0.3333333333333333703, 0.3170188387650512141, 0.3333333333333333703, 0.3170188387650512141, 0.3333333333333333703, 0.3170188387650512141, 0.3333333333333333703, 0.3170188387650512141, 0.3333333333333333703, 0.3170188387650512141, 0.3333333333333333703, 0.3170188387650512141, 0.3333333333333333703, 0.3170188387650512141, 0.3333333333333333703, 0.3170188387650512141, 0.3333333333333333703, 0.3170188387650512141, 0.3333333333333333703, 0.3170188387650512141, 0.3333333333333333703, 0.3170188387650512141, 0.3333333333333333703, 0.3170188387650512141, 0.3333333333333333703, 0.3170188387650512141, 0.3333333333333333703, 0.3170188387650512141, 0.3333333333333333703, 0.3170188387650512141, 0.3333333333333333703, 0.3170188387650512141, 0.3333333333333333703, 0.3170188387650512141, 0.3333333333333333703, 0.3170188387650512141, 0.3333333333333333703, 0.3170188387650512141, 0.3333333333333333703, 0.3170188387650512141, 0.3333333333333333703, 0.3170188387650512141, 0.3333333333333333703, 0.3170188387650512141, 0.3333333333333333703, 0.3170188387650512141, 0.3333333333333333703, 0.3170188387650512141, 0.3333333333333333703, 0.3170188387650512141, 0.3333333333333333703, 0.3170188387650512141, 0.3333333333333333703, 0.3170188387650512141, 0.3333333333333333703, 0.3170188387650512141, 0.3333333333333333703, 0.3170188387650512141, 0.3333333333333333703, 0.3170188387650512141, 0.3333333333333333703, 0.3170188387650512141, 0.3333333333333333703, 0.3170188387650512141, 0.3333333333333333703, 0.3170188387650512141, 0.3333333333333333703, 0.3170188387650512141, 0.3333333333333333703, 0.3170188387650512141, 0.3333333333333333703, 0.3170188387650512141, 0.3333333333333333703, 0.3170188387650512141, 0.3333333333333333703, 0.3170188387650512141, 0.3333333333333333703, 0.3170188387650512141, 0.3333333333333333703, 0.3170188387650512141, 0.3333333333333333703, 0.3170188387650512141, 0.3333333333333333703, 0.3170188387650512141, 0.3333333333333333703, 0.3170188387650512141, 0.3333333333333333703, 0.3170188387650512141, 0.3333333333333333703, 0.3170188387650512141, 0.3333333333333333703, 0.3170188387650512141, 0.3333333333333333703, 0.3170188387650512141, 0.3333333333333333703, 0.3170188387650512141, 0.3333333333333333703, 0.3170188387650512141, 0.3333333333333333703, 0.3170188387650512141, 0.3333333333333333703, 0.3170188387650512141, 0.3333333333333333703, 0.3170188387650512141, 0.3333333333333333703, 0.3170188387650512141, 0.3333333333333333703, 0.3170188387650512141, 0.3333333333333333703, 0.3170188387650512141, 0.3333333333333333703, 0.3170188387650512141, 0.3333333333333333703, 0.3170188387650512141, 0.3333333333333333703, 0.3170188387650512141, 0.3333333333333333703, 0.3170188387650512141, 0.3333333333333333703, 0.3170188387650512141, 0.3333333333333333703, 0.3170188387650512141, 0.3333333333333333703, 0.3170188387650512141, 0.3333333333333333703, 0.3170188387650512141, 0.3333333333333333703, 0.3170188387650512141, 0.3333333333333333703, 0.3170188387650512141, 0.3333333333333333703, 0.3170188387650512141, 0.3333333333333333703, 0.3170188387650512141, 0.3333333333333333703, 0.3170188387650512141, 0.3333333333333333703, 0.3170188387650512141, 0.3333333333333333703, 0.3170188387650512141, 0.3333333333333333703, 0.3170188387650512141, 0.3333333333333333703, 0.3170188387650512141, 0.3333333333333333703, 0.3170188387650512141, 0.3333333333333333703, 0.3170188387650512141, 0.3333333333333333703, 0.3170188387650512141, 0.3333333333333333703, 0.3170188387650512141, 0.3333333333333333703, 0.3170188387650512141, 0.3333333333333333703, 0.3170188387650512141, 0.3333333333333333703, 0.3170188387650512141, 0.3333333333333333703, 0.3170188387650512141, 0.3333333333333333703, 0.3170188387650512141, 0.3333333333333333703, 0.3170188387650512141, 0.3333333333333333703, 0.3170188387650512141, 0.3333333333333333703),
 ( 1.000000000000000000, 0.9510565162951535312, 1.000000000000000000, 0.9510565162951535312, 1.000000000000000000, 0.9510565162951535312, 1.000000000000000000, 0.9510565162951535312, 1.000000000000000000, 0.9510565162951535312, 1.000000000000000000, 0.9510565162951535312, 1.000000000000000000, 0.9510565162951535312, 1.000000000000000000, 0.9510565162951535312, 1.000000000000000000, 0.9510565162951535312, 1.000000000000000000, 0.9510565162951535312, 1.000000000000000000, 0.9510565162951535312, 1.000000000000000000, 0.9510565162951535312, 1.000000000000000000, 0.9510565162951535312, 1.000000000000000000, 0.9510565162951535312, 1.000000000000000000, 0.9510565162951535312, 1.000000000000000000, 0.9510565162951535312, 1.000000000000000000, 0.9510565162951535312, 1.000000000000000000, 0.9510565162951535312, 1.000000000000000000, 0.9510565162951535312, 1.000000000000000000, 0.9510565162951535312, 1.000000000000000000, 0.9510565162951535312, 1.000000000000000000, 0.9510565162951535312, 1.000000000000000000, 0.9510565162951535312, 1.000000000000000000, 0.9510565162951535312, 1.000000000000000000, 0.9510565162951535312, 1.000000000000000000, 0.9510565162951535312, 1.000000000000000000, 0.9510565162951535312, 1.000000000000000000, 0.9510565162951535312, 1.000000000000000000, 0.9510565162951535312, 1.000000000000000000, 0.9510565162951535312, 1.000000000000000000, 0.9510565162951535312, 1.000000000000000000, 0.9510565162951535312, 1.000000000000000000, 0.9510565162951535312, 1.000000000000000000, 0.9510565162951535312, 1.000000000000000000, 0.9510565162951535312, 1.000000000000000000, 0.9510565162951535312, 1.000000000000000000, 0.9510565162951535312, 1.000000000000000000, 0.9510565162951535312, 1.000000000000000000, 0.9510565162951535312, 1.000000000000000000, 0.9510565162951535312, 1.000000000000000000, 0.9510565162951535312, 1.000000000000000000, 0.9510565162951535312, 1.000000000000000000, 0.9510565162951535312, 1.000000000000000000, 0.9510565162951535312, 1.000000000000000000, 0.9510565162951535312, 1.000000000000000000, 0.9510565162951535312, 1.000000000000000000, 0.9510565162951535312, 1.000000000000000000, 0.9510565162951535312, 1.000000000000000000, 0.9510565162951535312, 1.000000000000000000, 0.9510565162951535312, 1.000000000000000000, 0.9510565162951535312, 1.000000000000000000, 0.9510565162951535312, 1.000000000000000000, 0.9510565162951535312, 1.000000000000000000, 0.9510565162951535312, 1.000000000000000000, 0.9510565162951535312, 1.000000000000000000, 0.9510565162951535312, 1.000000000000000000, 0.9510565162951535312, 1.000000000000000000, 0.9510565162951535312, 1.000000000000000000, 0.9510565162951535312, 1.000000000000000000, 0.9510565162951535312, 1.000000000000000000, 0.9510565162951535312, 1.000000000000000000, 0.9510565162951535312, 1.000000000000000000, 0.9510565162951535312, 1.000000000000000000, 0.9510565162951535312, 1.000000000000000000, 0.9510565162951535312, 1.000000000000000000, 0.9510565162951535312, 1.000000000000000000, 0.9510565162951535312, 1.000000000000000000, 0.9510565162951535312, 1.000000000000000000, 0.9510565162951535312, 1.000000000000000000, 0.9510565162951535312, 1.000000000000000000, 0.9510565162951535312, 1.000000000000000000, 0.9510565162951535312, 1.000000000000000000, 0.9510565162951535312, 1.000000000000000000, 0.9510565162951535312, 1.000000000000000000, 0.9510565162951535312, 1.000000000000000000, 0.9510565162951535312, 1.000000000000000000, 0.9510565162951535312, 1.000000000000000000, 0.9510565162951535312, 1.000000000000000000, 0.9510565162951535312, 1.000000000000000000, 0.9510565162951535312, 1.000000000000000000, 0.9510565162951535312, 1.000000000000000000, 0.9510565162951535312, 1.000000000000000000, 0.9510565162951535312, 1.000000000000000000, 0.9510565162951535312, 1.000000000000000000, 0.9510565162951535312, 1.000000000000000000, 0.9510565162951535312, 1.000000000000000000, 0.9510565162951535312, 1.000000000000000000, 0.9510565162951535312, 1.000000000000000000, 0.9510565162951535312, 1.000000000000000000, 0.9510565162951535312, 1.000000000000000000, 0.9510565162951535312, 1.000000000000000000, 0.9510565162951535312, 1.000000000000000000, 0.9510565162951535312, 1.000000000000000000, 0.9510565162951535312, 1.000000000000000000, 0.9510565162951535312, 1.000000000000000000, 0.9510565162951535312, 1.000000000000000000, 0.9510565162951535312, 1.000000000000000000, 0.9510565162951535312, 1.000000000000000000, 0.9510565162951535312, 1.000000000000000000, 0.9510565162951535312, 1.000000000000000000) ) ) 
 REPRESENTATION_ITEM ( '' )  SURFACE ( )  );
#8558 = DIRECTION ( 'NONE',  ( 1.000000000000000000, 0.000000000000000000, 0.000000000000000000 ) ) ;
#8559 = CARTESIAN_POINT ( 'NONE',  ( 52.57664461997811856, 45.59948385550240602, -8.007379884777229506 ) ) ;
#8560 = SURFACE_STYLE_FILL_AREA ( #18877 ) ;
#8561 = CARTESIAN_POINT ( 'NONE',  ( 44.05948171654945611, 46.20051614449766930, -4.345558710429044069 ) ) ;
#8562 = DIRECTION ( 'NONE',  ( 0.000000000000000000, 0.000000000000000000, -1.000000000000000000 ) ) ;
#8564 = ORIENTED_EDGE ( 'NONE', *, *, #10750, .T. ) ;
#8563 = ADVANCED_FACE ( 'NONE', ( #9464 ), #9000, .T. ) ;
#8565 = EDGE_CURVE ( 'NONE', #6708, #6185, #12499, .T. ) ;
#8566 = ORIENTED_EDGE ( 'NONE', *, *, #3062, .T. ) ;
#8567 = DIRECTION ( 'NONE',  ( -1.000000000000000000, 0.000000000000000000, 0.000000000000000000 ) ) ;
#8568 = ORIENTED_EDGE ( 'NONE', *, *, #6883, .T. ) ;
#8569 = DIRECTION ( 'NONE',  ( 0.000000000000000000, 0.000000000000000000, 1.000000000000000000 ) ) ;
#8570 = ORIENTED_EDGE ( 'NONE', *, *, #18647, .T. ) ;
#8571 = DIRECTION ( 'NONE',  ( -1.000000000000000000, 0.000000000000000000, 0.000000000000000000 ) ) ;
#8572 = ADVANCED_FACE ( 'NONE', ( #9841 ), #2426, .F. ) ;
#8573 = EDGE_LOOP ( 'NONE', ( #8415, #13227 ) ) ;
#8574 = DIRECTION ( 'NONE',  ( 0.000000000000000000, 0.000000000000000000, 1.000000000000000000 ) ) ;
#8575 = ORIENTED_EDGE ( 'NONE', *, *, #1556, .F. ) ;
#8576 = CARTESIAN_POINT ( 'NONE',  ( 54.72065718078924590, 56.29948385550240886, 6.458785618021043895 ) ) ;
#8577 = CARTESIAN_POINT ( 'NONE',  ( 0.000000000000000000, 3.031088913245533423, -1.750000000000004885 ) ) ;
#8578 = CARTESIAN_POINT ( 'NONE',  ( 53.54508667620428497, 50.29948385550240886, 4.840751629271157874 ) ) ;
#8579 = DIRECTION ( 'NONE',  ( -0.000000000000000000, 1.000000000000000000, -0.000000000000000000 ) ) ;
#8580 = CARTESIAN_POINT ( 'NONE',  ( 6.534838248920897819, 2.951765777552412651, 5.112608298763836601 ) ) ;
#8581 = CARTESIAN_POINT ( 'NONE',  ( 47.74827507625469281, 64.40051614449765793, -7.007379884777203749 ) ) ;
#8582 = AXIS2_PLACEMENT_3D ( 'NONE', #7429, #7524, #3026 ) ;
#8583 = CARTESIAN_POINT ( 'NONE',  ( 43.69122665457040000, 50.00051614449765935, -0.02388180880515696977 ) ) ;
#8584 = CARTESIAN_POINT ( 'NONE',  ( -6.259644161404862988E-16, -4.618802153517027165, -3.504271511726793076 ) ) ;
#8585 = DIRECTION ( 'NONE',  ( -1.000000000000000000, -1.387778780781445182E-16, -0.000000000000000000 ) ) ;
#8586 = ORIENTED_EDGE ( 'NONE', *, *, #2312, .F. ) ;
#8587 = VERTEX_POINT ( 'NONE', #1230 ) ;
#8588 = CARTESIAN_POINT ( 'NONE',  ( -2.682243648011671588, -3.070208061305317759, -0.04852650426602272971 ) ) ;
#8589 = FILL_AREA_STYLE ('',( #9041 ) ) ;
#8590 = ORIENTED_EDGE ( 'NONE', *, *, #10467, .F. ) ;
#8591 = CARTESIAN_POINT ( 'NONE',  ( 42.63976443033212860, 58.99948385550239038, 0.02388180880522514787 ) ) ;
#8592 = CARTESIAN_POINT ( 'NONE',  ( 3.973110223768738791, 0.6864646529411682074, 3.565797985667475967 ) ) ;
#8593 = ORIENTED_EDGE ( 'NONE', *, *, #9162, .F. ) ;
#8594 = ORIENTED_EDGE ( 'NONE', *, *, #12633, .T. ) ;
#8595 = CARTESIAN_POINT ( 'NONE',  ( -154.9999999999999716, -14.99999999999999645, 3.999999999999999112 ) ) ;
#8596 = CARTESIAN_POINT ( 'NONE',  ( -54.99999999999996447, -14.99999999999998579, 10.00000000000000000 ) ) ;
#8597 = VERTEX_POINT ( 'NONE', #16045 ) ;
#8598 = CARTESIAN_POINT ( 'NONE',  ( 17.79870116617255604, -29.12174527145369396, 0.000000000000000000 ) ) ;
#8599 = ORIENTED_EDGE ( 'NONE', *, *, #773, .F. ) ;
#8600 = FACE_OUTER_BOUND ( 'NONE', #18595, .T. ) ;
#8601 = CARTESIAN_POINT ( 'NONE',  ( 52.25172492374522903, 49.59948385550240602, -7.007379884777225953 ) ) ;
#8602 = CARTESIAN_POINT ( 'NONE',  ( 0.1713913650100259145, 0.000000000000000000, 4.424999999999999822 ) ) ;
#8603 = CARTESIAN_POINT ( 'NONE',  ( 45.90387839640208512, 48.30051614449765651, -5.676469297603124353 ) ) ;
#8604 = PLANE ( 'NONE',  #15820 ) ;
#8605 = ADVANCED_FACE ( 'NONE', ( #2530 ), #7008, .F. ) ;
#8606 = FILL_AREA_STYLE ('',( #15776 ) ) ;
#8607 = CARTESIAN_POINT ( 'NONE',  ( -4.158233816355195955, -0.4370479853238878887, 9.000000000000000000 ) ) ;
#8608 = AXIS2_PLACEMENT_3D ( 'NONE', #14797, #16576, #1374 ) ;
#8609 = ADVANCED_FACE ( 'NONE', ( #17710 ), #16840, .F. ) ;
#8610 = ORIENTED_EDGE ( 'NONE', *, *, #6870, .F. ) ;
#8611 = EDGE_LOOP ( 'NONE', ( #5459, #5849, #3868, #9281 ) ) ;
#8612 = CARTESIAN_POINT ( 'NONE',  ( 4.175813232069148562, 4.122719923832741884, -2.765695189283172261E-17 ) ) ;
#8613=STYLED_ITEM('',(#19482),#8823);
#8614 = CARTESIAN_POINT ( 'NONE',  ( -17.79870116617248499, -10.87825472854618170, 0.000000000000000000 ) ) ;
#8615 = CARTESIAN_POINT ( 'NONE',  ( 2.649999999999988365, 15.00000000000001599, -9.999999999999998224 ) ) ;
#8616 = ORIENTED_EDGE ( 'NONE', *, *, #15670, .F. ) ;
#8617 = DIRECTION ( 'NONE',  ( -0.9135454576426043083, 0.4067366430757925477, 0.000000000000000000 ) ) ;
#8618 = VERTEX_POINT ( 'NONE', #14464 ) ;
#8619 = VERTEX_POINT ( 'NONE', #1427 ) ;
#8620 = DIRECTION ( 'NONE',  ( 0.000000000000000000, 0.000000000000000000, -1.000000000000000000 ) ) ;
#8621 = CARTESIAN_POINT ( 'NONE',  ( -5.384454397937118664, 6.702023979852544604E-16, -5.000000000000000000 ) ) ;
#8622 = CARTESIAN_POINT ( 'NONE',  ( 55.71335778527780036, 48.90051614449766504, -1.832500667257213056 ) ) ;
#8623 = CARTESIAN_POINT ( 'NONE',  ( -8.134732861515892921, -38.27090915285207018, -9.000000000000000000 ) ) ;
#8624 = CIRCLE ( 'NONE', #2699, 20.00000000000000000 ) ;
#8625 = CYLINDRICAL_SURFACE ( 'NONE', #18423, 2.000000000000000888 ) ;
#8626 = CARTESIAN_POINT ( 'NONE',  ( 44.30067958973596376, 50.89948385550240317, 1.875703265242204099 ) ) ;
#8627 = DIRECTION ( 'NONE',  ( -0.000000000000000000, -0.000000000000000000, 1.000000000000000000 ) ) ;
#8628 = CARTESIAN_POINT ( 'NONE',  ( 47.37792948025162332, 63.39948385550238896, -7.992620115222770494 ) ) ;
#8629 = CARTESIAN_POINT ( 'NONE',  ( 45.27934281921082516, 47.70051614449766220, 6.458785618021089192 ) ) ;
#8630 = CARTESIAN_POINT ( 'NONE',  ( 4.175572532730932096, -2.061029303918058275, -3.569807470274390493 ) ) ;
#8631 = VECTOR ( 'NONE', #8406, 1000.000000000000000 ) ;
#8632 = ORIENTED_EDGE ( 'NONE', *, *, #960, .T. ) ;
#8633 = DIRECTION ( 'NONE',  ( -0.000000000000000000, -0.000000000000000000, 1.000000000000000000 ) ) ;
#8634 = APPLICATION_PROTOCOL_DEFINITION ( 'draft international standard', 'automotive_design', 1998, #17808 ) ;
#8635 = ORIENTED_EDGE ( 'NONE', *, *, #4734, .F. ) ;
#8636 = CARTESIAN_POINT ( 'NONE',  ( -2.836893136758495970, -3.208949435745868328, -3.505054077164885484 ) ) ;
#8637 = CIRCLE ( 'NONE', #3333, 1.000000000000000444 ) ;
#8638 = CARTESIAN_POINT ( 'NONE',  ( -7.134732861515892033, -38.27090915285207018, -9.000000000000000000 ) ) ;
#8639 = DIRECTION ( 'NONE',  ( 1.000000000000000000, 0.000000000000000000, 0.000000000000000000 ) ) ;
#8640 = AXIS2_PLACEMENT_3D ( 'NONE', #3733, #17470, #8232 ) ;
#8641 = FACE_OUTER_BOUND ( 'NONE', #10654, .T. ) ;
#8642 = ORIENTED_EDGE ( 'NONE', *, *, #17618, .F. ) ;
#8643 = CARTESIAN_POINT ( 'NONE',  ( -154.8605857259444463, -18.79744172571344762, 15.79999999999999893 ) ) ;
#8644 = EDGE_CURVE ( 'NONE', #5816, #6699, #4634, .T. ) ;
#8645 = DIRECTION ( 'NONE',  ( 0.000000000000000000, 0.000000000000000000, 1.000000000000000000 ) ) ;
#8646 = CARTESIAN_POINT ( 'NONE',  ( 43.33558569842703179, 51.09948385550240602, -2.141517661632099223 ) ) ;
#8647 = CARTESIAN_POINT ( 'NONE',  ( -154.9999999999999716, -14.99999999999999645, -15.00000000000000000 ) ) ;
#8648 = CARTESIAN_POINT ( 'NONE',  ( 47.37792948025162332, 47.39948385550241028, -7.992620115222770494 ) ) ;
#8649 = PLANE ( 'NONE',  #3821 ) ;
#8650 = CARTESIAN_POINT ( 'NONE',  ( 47.70284917648459100, 49.60051614449763946, 6.992620115222796251 ) ) ;
#8651 = APPLICATION_CONTEXT ( 'automotive_design' ) ;
#8652 = DIRECTION ( 'NONE',  ( 0.000000000000000000, 0.000000000000000000, 1.000000000000000000 ) ) ;
#8653 = ORIENTED_EDGE ( 'NONE', *, *, #13461, .F. ) ;
#8654 = VERTEX_POINT ( 'NONE', #8768 ) ;
#8655 = DIRECTION ( 'NONE',  ( -1.000000000000000000, 0.000000000000000000, 0.000000000000000000 ) ) ;
#8656 = ORIENTED_EDGE ( 'NONE', *, *, #5000, .F. ) ;
#8657 = DIRECTION ( 'NONE',  ( 0.000000000000000000, 0.000000000000000000, -1.000000000000000000 ) ) ;
#8658 = EDGE_CURVE ( 'NONE', #16221, #2254, #18106, .T. ) ;
#8659 = AXIS2_PLACEMENT_3D ( 'NONE', #6877, #7255, #13229 ) ;
#8660 = ORIENTED_EDGE ( 'NONE', *, *, #9258, .T. ) ;
#8661 = CARTESIAN_POINT ( 'NONE',  ( 4.101954839143060028, 2.368264730582927857, -3.681130640444267854 ) ) ;
#8662 = ORIENTED_EDGE ( 'NONE', *, *, #8673, .T. ) ;
#8663 = DIRECTION ( 'NONE',  ( 1.000000000000000000, 0.000000000000000000, 0.000000000000000000 ) ) ;
#8664 = VERTEX_POINT ( 'NONE', #11804 ) ;
#8665 = SHAPE_REPRESENTATION ( 'reel holder', ( #10359 ), #2171 ) ;
#8666 = CARTESIAN_POINT ( 'NONE',  ( 58.41169779390614281, 59.99948385550241170, -0.02388180880523160798 ) ) ;
#8667 = B_SPLINE_CURVE_WITH_KNOTS ( 'NONE', 3,
 ( #18403, #15533, #9350, #13581, #17024, #443 ),
 .UNSPECIFIED., .F., .F.,
 ( 4, 2, 4 ),
 ( 0.000000000000000000, 0.002086519881787261485, 0.004173039763574522970 ),
 .UNSPECIFIED. ) ;
#8668 = ADVANCED_FACE ( 'NONE', ( #4364 ), #18995, .F. ) ;
#8669 = AXIS2_PLACEMENT_3D ( 'NONE', #1785, #593, #18174 ) ;
#8670 = CARTESIAN_POINT ( 'NONE',  ( 48.07319477248768180, 48.59948385550239891, 6.007379884777225953 ) ) ;
#8672 = EDGE_CURVE ( 'NONE', #14431, #11986, #1134, .T. ) ;
#8671 = DIRECTION ( 'NONE',  ( 0.000000000000000000, 0.000000000000000000, 1.000000000000000000 ) ) ;
#8673 = EDGE_CURVE ( 'NONE', #15764, #6353, #17775, .T. ) ;
#8674 = DIRECTION ( 'NONE',  ( 1.000000000000000000, 0.000000000000000000, 0.000000000000000000 ) ) ;
#8675 = CARTESIAN_POINT ( 'NONE',  ( 49.97728705011495265, 49.50051614449766646, 8.000000000000001776 ) ) ;
#8676 = CARTESIAN_POINT ( 'NONE',  ( 44.88205777487401349, 49.80051614449765651, 3.688883143319584779 ) ) ;
#8677 = AXIS2_PLACEMENT_3D ( 'NONE', #14351, #10614, #4557 ) ;
#8678 = CARTESIAN_POINT ( 'NONE',  ( -158.7997795378487353, -15.04093242902330907, -15.00000000000000000 ) ) ;
#8679 = AXIS2_PLACEMENT_3D ( 'NONE', #476, #10671, #18248 ) ;
#8680 = CARTESIAN_POINT ( 'NONE',  ( -1.999999999999999556, 3.464101615137754830, -3.142992957459232795 ) ) ;
#8681 = ORIENTED_EDGE ( 'NONE', *, *, #1028, .T. ) ;
#8682 = EDGE_CURVE ( 'NONE', #10736, #7530, #7401, .T. ) ;
#8683 = VERTEX_POINT ( 'NONE', #5834 ) ;
#8684 = DIRECTION ( 'NONE',  ( -0.000000000000000000, 1.000000000000000000, -0.000000000000000000 ) ) ;
#8685 = VERTEX_POINT ( 'NONE', #18901 ) ;
#8686 = CARTESIAN_POINT ( 'NONE',  ( 44.03140696652192787, 57.19948385550238612, -4.306917132069425058 ) ) ;
#8687 = LINE ( 'NONE', #12010, #3737 ) ;
#8688 = VECTOR ( 'NONE', #5292, 1000.000000000000000 ) ;
#8689 = VERTEX_POINT ( 'NONE', #8580 ) ;
#8690 = ORIENTED_EDGE ( 'NONE', *, *, #2207, .T. ) ;
#8691 = CARTESIAN_POINT ( 'NONE',  ( 1.000000000000000000, -5.408326913195983465, 0.000000000000000000 ) ) ;
#8692 = LINE ( 'NONE', #73, #15975 ) ;
#8693 = ORIENTED_EDGE ( 'NONE', *, *, #4229, .F. ) ;
#8694 = DIRECTION ( 'NONE',  ( -0.000000000000000000, -0.000000000000000000, 1.000000000000000000 ) ) ;
#8695 = ORIENTED_EDGE ( 'NONE', *, *, #2763, .T. ) ;
#8696 = CARTESIAN_POINT ( 'NONE',  ( -2.725741868435985094, 3.045094352034055429, -3.220599429844047012 ) ) ;
#8697 = EDGE_CURVE ( 'NONE', #1643, #1761, #5439, .T. ) ;
#8698 = CARTESIAN_POINT ( 'NONE',  ( 44.03140696652192787, 53.19948385550238612, -4.306917132069425058 ) ) ;
#8699 = ADVANCED_FACE ( 'NONE', ( #11415 ), #7104, .T. ) ;
#8700 = CARTESIAN_POINT ( 'NONE',  ( 2.899426713160750069, -23.82535289025860337, -8.999999999999996447 ) ) ;
#8701 = CARTESIAN_POINT ( 'NONE',  ( 54.09612160359792199, 45.30051614449766362, 5.676469297603124353 ) ) ;
#8702 = DIRECTION ( 'NONE',  ( 0.02857142857142857401, 0.9995917534020515305, -0.000000000000000000 ) ) ;
#8703 = DIRECTION ( 'NONE',  ( 0.000000000000000000, 0.000000000000000000, 1.000000000000000000 ) ) ;
#8704 = AXIS2_PLACEMENT_3D ( 'NONE', #10791, #9322, #5013 ) ;
#8705 = ORIENTED_EDGE ( 'NONE', *, *, #18085, .T. ) ;
#8706 = VERTEX_POINT ( 'NONE', #16333 ) ;
#8707 = FACE_BOUND ( 'NONE', #10738, .T. ) ;
#8708 = SHAPE_REPRESENTATION_RELATIONSHIP ( 'NONE' , 'NONE' ,  #13428, #7556 ) ;
#8709 = DIRECTION ( 'NONE',  ( 0.000000000000000000, 0.000000000000000000, 1.000000000000000000 ) ) ;
#8710 = DIRECTION ( 'NONE',  ( -0.9995235871707960351, -0.03086419753086420970, 0.000000000000000000 ) ) ;
#8711 = VERTEX_POINT ( 'NONE', #17419 ) ;
#8712 = CARTESIAN_POINT ( 'NONE',  ( 6.390983399715593372, 5.837459000499768180, -0.1107755759658281131 ) ) ;
#8713 = EDGE_CURVE ( 'NONE', #18086, #2296, #10869, .T. ) ;
#8714 = ORIENTED_EDGE ( 'NONE', *, *, #7718, .T. ) ;
#8715 = ORIENTED_EDGE ( 'NONE', *, *, #423, .T. ) ;
#8716 = EDGE_CURVE ( 'NONE', #9785, #4866, #13186, .T. ) ;
#8717 = CIRCLE ( 'NONE', #1827, 4.000000000000031086 ) ;
#8718 = CYLINDRICAL_SURFACE ( 'NONE', #2225, 4.424999999999999822 ) ;
#8719 = PRODUCT_DEFINITION_CONTEXT ( 'detailed design', #6286, 'design' ) ;
#8720 = EDGE_CURVE ( 'NONE', #15947, #14101, #16856, .T. ) ;
#8721 = CARTESIAN_POINT ( 'NONE',  ( 49.97728705011494554, 47.50051614449765935, 6.000000000000000888 ) ) ;
#8722 = CARTESIAN_POINT ( 'NONE',  ( 2.449293598294706513E-15, -20.00000000000000000, -23.00000000000000000 ) ) ;
#8723 = DIRECTION ( 'NONE',  ( 0.1045284632676494602, 0.9945218953682738450, 0.000000000000000000 ) ) ;
#8724 = CARTESIAN_POINT ( 'NONE',  ( 48.07319477248768180, 50.59948385550240602, 6.007379884777225953 ) ) ;
#8725 = PLANE ( 'NONE',  #16025 ) ;
#8726 = CARTESIAN_POINT ( 'NONE',  ( 57.36023556966787851, 49.99948385550238328, -0.02388180880522424582 ) ) ;
#8727 = CARTESIAN_POINT ( 'NONE',  ( 54.68390685589039890, 45.30051614449766362, 6.485486291978072693 ) ) ;
#8728 = CARTESIAN_POINT ( 'NONE',  ( 0.08165819712376803929, -3.720292241887084295, 3.556264818047238041 ) ) ;
#8729 = VERTEX_POINT ( 'NONE', #7203 ) ;
#8730 = DIRECTION ( 'NONE',  ( 1.000000000000000000, 0.000000000000000000, -0.000000000000000000 ) ) ;
#8731 =( NAMED_UNIT ( * ) SI_UNIT ( $, .STERADIAN. ) SOLID_ANGLE_UNIT ( ) );
#8732=STYLED_ITEM('',(#19454),#15430);
#8733 = AXIS2_PLACEMENT_3D ( 'NONE', #1845, #16752, #13792 ) ;
#8734 = EDGE_LOOP ( 'NONE', ( #17536, #18258, #2736, #15788, #14951, #19210, #8898, #14886, #12932, #18010, #15244, #19234, #12730, #4569, #9076, #7118, #15263, #18210, #19137, #4571 ) ) ;
#8735 = CARTESIAN_POINT ( 'NONE',  ( 1.267864665261691752E-11, -20.00000000000000000, 9.999999999999998224 ) ) ;
#8736 = EDGE_CURVE ( 'NONE', #6664, #1514, #11703, .T. ) ;
#8737 = CARTESIAN_POINT ( 'NONE',  ( 3.175194142251945184, -0.2536549670829196801, -9.000000000000000000 ) ) ;
#8738 = EDGE_CURVE ( 'NONE', #15388, #18444, #6124, .T. ) ;
#8739 = FACE_OUTER_BOUND ( 'NONE', #18556, .T. ) ;
#8740 = CARTESIAN_POINT ( 'NONE',  ( 6.367873360227556567, 2.886751345948125991, 4.999999999999999112 ) ) ;
#8741 = CARTESIAN_POINT ( 'NONE',  ( 62.49999999999998579, 40.00000000000001421, 5.000000000000000000 ) ) ;
#8742 = DIRECTION ( 'NONE',  ( -1.000000000000000000, 0.000000000000000000, 0.000000000000000000 ) ) ;
#8743 = AXIS2_PLACEMENT_3D ( 'NONE', #6227, #16638, #12201 ) ;
#8744 = DIRECTION ( 'NONE',  ( -0.2439756946365075896, 0.9697813467099857254, 1.610118993450814692E-22 ) ) ;
#8745 = CARTESIAN_POINT ( 'NONE',  ( 47.70284917648453415, 53.39948385550238186, -6.992620115222774047 ) ) ;
#8746 = CARTESIAN_POINT ( 'NONE',  ( 20.00000000000000000, -20.00000000000000000, -23.00000000000000000 ) ) ;
#8747 = CARTESIAN_POINT ( 'NONE',  ( 43.20883090819745576, 54.79948385550240175, 4.963592699179006473 ) ) ;
#8748 = CARTESIAN_POINT ( 'NONE',  ( -4.000000000000000000, 2.309401076758498483, -3.433295621305379353 ) ) ;
#8749 = CARTESIAN_POINT ( 'NONE',  ( 47.70284917648459100, 45.60051614449765367, 6.992620115222796251 ) ) ;
#8750 = AXIS2_PLACEMENT_3D ( 'NONE', #15846, #17523, #2432 ) ;
#8751 = CARTESIAN_POINT ( 'NONE',  ( -19.30627432446647518, -14.77814480204147785, -9.000000000000000000 ) ) ;
#8752 = ORIENTED_EDGE ( 'NONE', *, *, #9762, .F. ) ;
#8753 = VERTEX_POINT ( 'NONE', #15137 ) ;
#8754 = DIRECTION ( 'NONE',  ( 0.000000000000000000, 0.000000000000000000, 1.000000000000000000 ) ) ;
#8755 = ORIENTED_EDGE ( 'NONE', *, *, #7238, .F. ) ;
#8756 = AXIS2_PLACEMENT_3D ( 'NONE', #12569, #15807, #11085 ) ;
#8757 = CYLINDRICAL_SURFACE ( 'NONE', #5942, 2.000000000000001776 ) ;
#8758 = VERTEX_POINT ( 'NONE', #19398 ) ;
#8759 = CARTESIAN_POINT ( 'NONE',  ( 20.00000000000000000, -20.00000000000000000, -20.00000000000000000 ) ) ;
#8760 = VERTEX_POINT ( 'NONE', #11999 ) ;
#8761 = AXIS2_PLACEMENT_3D ( 'NONE', #4471, #15432, #5040 ) ;
#8762 = LINE ( 'NONE', #7490, #12733 ) ;
#8763 = ORIENTED_EDGE ( 'NONE', *, *, #763, .T. ) ;
#8764 = CARTESIAN_POINT ( 'NONE',  ( 54.68390685589033495, 57.69948385550241454, -6.485486291978119766 ) ) ;
#8765 = DIRECTION ( 'NONE',  ( 1.000000000000000000, 0.000000000000000000, 0.000000000000000000 ) ) ;
#8766 = CARTESIAN_POINT ( 'NONE',  ( 53.50833635130540955, 57.69948385550241454, -4.867452303228209765 ) ) ;
#8767 = DIRECTION ( 'NONE',  ( 1.000000000000000000, 0.000000000000000000, -0.000000000000000000 ) ) ;
#8768 = CARTESIAN_POINT ( 'NONE',  ( -16.79901371501587803, -9.146745271453902149, -9.000000000000000000 ) ) ;
#8769 = APPLICATION_CONTEXT ( 'automotive_design' ) ;
#8770 = CARTESIAN_POINT ( 'NONE',  ( 52.57664461997821093, 49.40051614449766504, 8.007379884777206414 ) ) ;
#8771 = CIRCLE ( 'NONE', #10008, 4.424999999999999822 ) ;
#8772 = CARTESIAN_POINT ( 'NONE',  ( 43.69122665457040000, 52.00051614449766646, -0.02388180880515696977 ) ) ;
#8774 = AXIS2_PLACEMENT_3D ( 'NONE', #8116, #17153, #12433 ) ;
#8773 = CARTESIAN_POINT ( 'NONE',  ( 4.200000000000001954, 0.000000000000000000, 0.000000000000000000 ) ) ;
#8775 = AXIS2_PLACEMENT_3D ( 'NONE', #6136, #12107, #253 ) ;
#8776 = DIRECTION ( 'NONE',  ( 0.000000000000000000, 0.000000000000000000, 1.000000000000000000 ) ) ;
#8777 = VERTEX_POINT ( 'NONE', #7682 ) ;
#8778 = CONICAL_SURFACE ( 'NONE', #1903, 3.309499999999999886, 0.7853981633974407295 ) ;
#8779 = VERTEX_POINT ( 'NONE', #3278 ) ;
#8780 = CARTESIAN_POINT ( 'NONE',  ( -3.679171394226034675, -2.494631558665844739, -0.3503314178412558211 ) ) ;
#8781 = ORIENTED_EDGE ( 'NONE', *, *, #9024, .T. ) ;
#8782 = EDGE_CURVE ( 'NONE', #7530, #2523, #8013, .T. ) ;
#8783 = DIRECTION ( 'NONE',  ( 1.000000000000000000, 0.000000000000000000, 0.000000000000000000 ) ) ;
#8784 = DIRECTION ( 'NONE',  ( 0.000000000000000000, 0.000000000000000000, -1.000000000000000000 ) ) ;
#8785 = ORIENTED_EDGE ( 'NONE', *, *, #16169, .T. ) ;
#8786 = CARTESIAN_POINT ( 'NONE',  ( -4.000000000000000000, 2.309401076758498483, -3.433295621305379353 ) ) ;
#8787 = PRODUCT_DEFINITION ( 'UNKNOWN', '', #12608, #1862 ) ;
#8788 = CARTESIAN_POINT ( 'NONE',  ( 2.354826896168714434, -6.962563485461402024, -1.000000000000000000 ) ) ;
#8789 = EDGE_CURVE ( 'NONE', #6353, #16243, #15273, .T. ) ;
#8790 = MANIFOLD_SOLID_BREP ( 'Body', #14303 ) ;
#8791 = ORIENTED_EDGE ( 'NONE', *, *, #9510, .T. ) ;
#8792 = VECTOR ( 'NONE', #6819, 1000.000000000000000 ) ;
#8793 = CARTESIAN_POINT ( 'NONE',  ( 12.54977455159136568, -35.57251292194775516, -9.000000000000000000 ) ) ;
#8794 = ORIENTED_EDGE ( 'NONE', *, *, #2872, .F. ) ;
#8795 = ADVANCED_FACE ( 'NONE', ( #9158 ), #12192, .F. ) ;
#8796 = ADVANCED_FACE ( 'NONE', ( #12291, #18100, #4662 ), #6318, .T. ) ;
#8797 = CARTESIAN_POINT ( 'NONE',  ( 45.86712807150323812, 51.29948385550240175, -5.649768623646098220 ) ) ;
#8798 = PLANE ( 'NONE',  #13380 ) ;
#8799 = COLOUR_RGB ( '',0.8941176470588234615, 0.8941176470588234615, 0.8941176470588234615 ) ;
#8800 = CARTESIAN_POINT ( 'NONE',  ( 45.86712807150329496, 49.70051614449766220, 5.649768623646139964 ) ) ;
#8801 = CARTESIAN_POINT ( 'NONE',  ( 73.00000000000002842, -1.000000000000000000, -5.999999999999998224 ) ) ;
#8802 = ADVANCED_FACE ( 'NONE', ( #10620 ), #1523, .T. ) ;
#8803 = DIRECTION ( 'NONE',  ( 0.000000000000000000, 0.000000000000000000, 1.000000000000000000 ) ) ;
#8804 = DIRECTION ( 'NONE',  ( 1.000000000000000000, 0.000000000000000000, 0.000000000000000000 ) ) ;
#8805 = CIRCLE ( 'NONE', #11301, 2.100000000000000089 ) ;
#8806 = EDGE_LOOP ( 'NONE', ( #8321, #8125, #3471, #14290, #16247, #10848, #17066 ) ) ;
#8807 = ORIENTED_EDGE ( 'NONE', *, *, #4975, .F. ) ;
#8808 = CARTESIAN_POINT ( 'NONE',  ( -0.6448876103708541807, -4.246476118072358474, -0.2256878752776773356 ) ) ;
#8809 = FILL_AREA_STYLE_COLOUR ( '', #12463 ) ;
#8810 = AXIS2_PLACEMENT_3D ( 'NONE', #18105, #12295, #4666 ) ;
#8811 = ADVANCED_FACE ( 'NONE', ( #4759 ), #10720, .F. ) ;
#8812 = CARTESIAN_POINT ( 'NONE',  ( 45.90387839640214196, 48.69948385550240744, 5.676469297603166098 ) ) ;
#8813 = EDGE_CURVE ( 'NONE', #11790, #6465, #9241, .T. ) ;
#8814 = LINE ( 'NONE', #10374, #9657 ) ;
#8815 = VERTEX_POINT ( 'NONE', #6035 ) ;
#8816 = DIRECTION ( 'NONE',  ( 0.3090169943749456194, 0.9510565162951541973, 0.000000000000000000 ) ) ;
#8817 = ORIENTED_EDGE ( 'NONE', *, *, #15749, .T. ) ;
#8818 = ORIENTED_EDGE ( 'NONE', *, *, #9144, .T. ) ;
#8819 = CYLINDRICAL_SURFACE ( 'NONE', #3166, 8.099999999999999645 ) ;
#8820 = CARTESIAN_POINT ( 'NONE',  ( 8.500000000000000000, 9.800365875394399578E-16, -7.900000000000002132 ) ) ;
#8821 = CARTESIAN_POINT ( 'NONE',  ( 44.91013252490150620, 50.20051614449766220, -3.727524721679154940 ) ) ;
#8822 = DIRECTION ( 'NONE',  ( 1.000000000000000000, -9.251858538542972814E-17, 0.000000000000000000 ) ) ;
#8823 = MANIFOLD_SOLID_BREP ( 'Cavity1', #5866 ) ;
#8824 = CARTESIAN_POINT ( 'NONE',  ( 62.49999999999998579, 45.00000000000001421, 15.00000000000000000 ) ) ;
#8825 = CIRCLE ( 'NONE', #382, 1.000000000000001554 ) ;
#8826 = CARTESIAN_POINT ( 'NONE',  ( 48.07319477248768180, 60.59948385550240602, 6.007379884777225953 ) ) ;
#8827 = CARTESIAN_POINT ( 'NONE',  ( 0.000000000000000000, 0.000000000000000000, 0.000000000000000000 ) ) ;
#8828 = CARTESIAN_POINT ( 'NONE',  ( 49.97728705011488159, 55.49948385550240459, -7.000000000000000888 ) ) ;
#8829 = CARTESIAN_POINT ( 'NONE',  ( 57.60143344285435774, 51.10051614449766078, 2.493737253992045044 ) ) ;
#8830 = DIRECTION ( 'NONE',  ( -0.000000000000000000, -0.000000000000000000, 1.000000000000000000 ) ) ;
#8831 = CARTESIAN_POINT ( 'NONE',  ( 3.958484000407829217, 2.327740518749080056, -2.968235154689852440 ) ) ;
#8832 = ORIENTED_EDGE ( 'NONE', *, *, #12671, .F. ) ;
#8833 = DIRECTION ( 'NONE',  ( 0.000000000000000000, 0.000000000000000000, 1.000000000000000000 ) ) ;
#8834 = DIRECTION ( 'NONE',  ( 0.000000000000000000, 0.000000000000000000, 1.000000000000000000 ) ) ;
#8835 = DIRECTION ( 'NONE',  ( 0.9873505073845697533, 0.1585527532634883052, 0.000000000000000000 ) ) ;
#8836 = ORIENTED_EDGE ( 'NONE', *, *, #5001, .F. ) ;
#8837 = DIRECTION ( 'NONE',  ( 0.000000000000000000, -1.000000000000000000, 0.000000000000000000 ) ) ;
#8838 = PRODUCT_DEFINITION_SHAPE ( 'NONE', 'NONE',  #19418 ) ;
#8839 = DIRECTION ( 'NONE',  ( 1.000000000000000000, 0.000000000000000000, 0.000000000000000000 ) ) ;
#8840 = CARTESIAN_POINT ( 'NONE',  ( -2.649999999999988365, 15.00000000000001599, 15.00000000000000000 ) ) ;
#8841 = CARTESIAN_POINT ( 'NONE',  ( -154.9999999999999716, -14.99999999999999645, 15.00000000000000000 ) ) ;
#8842 = DIRECTION ( 'NONE',  ( -0.000000000000000000, -0.000000000000000000, 1.000000000000000000 ) ) ;
#8843 = CARTESIAN_POINT ( 'NONE',  ( -158.7998746980210001, -15.03085902363206472, 15.79999999999999893 ) ) ;
#8844 = CARTESIAN_POINT ( 'NONE',  ( -1.566204647097437563, -6.822536405429463713, -0.8000000000000000444 ) ) ;
#8845 = CARTESIAN_POINT ( 'NONE',  ( 50.02271294988512551, 56.49948385550240459, 7.000000000000000888 ) ) ;
#8846 = VECTOR ( 'NONE', #2425, 1000.000000000000000 ) ;
#8847 = CARTESIAN_POINT ( 'NONE',  ( -3.160591952521660364, -3.281206521718067037, -0.8000000000000000444 ) ) ;
#8848 = CARTESIAN_POINT ( 'NONE',  ( 57.60143344285433642, 55.89948385550241028, -2.493737253992118319 ) ) ;
#8849 = CARTESIAN_POINT ( 'NONE',  ( 3.880206590543187950, -2.665671387532591474, -2.382921720510934538 ) ) ;
#8850 = CARTESIAN_POINT ( 'NONE',  ( 42.63976443033212860, 46.00051614449766646, -0.02388180880514948964 ) ) ;
#8851 = ADVANCED_FACE ( 'NONE', ( #18676 ), #16811, .T. ) ;
#8852 = PLANE ( 'NONE',  #13175 ) ;
#8853 = ORIENTED_EDGE ( 'NONE', *, *, #7653, .T. ) ;
#8854 = EDGE_CURVE ( 'NONE', #9539, #14839, #6595, .T. ) ;
#8855 = ORIENTED_EDGE ( 'NONE', *, *, #9867, .F. ) ;
#8856 = DIRECTION ( 'NONE',  ( -0.000000000000000000, -0.000000000000000000, -1.000000000000000000 ) ) ;
#8857 = VERTEX_POINT ( 'NONE', #6401 ) ;
#8858 = FACE_BOUND ( 'NONE', #15980, .T. ) ;
#8859 = EDGE_LOOP ( 'NONE', ( #18492, #16534, #11305, #356 ) ) ;
#8860 = LINE ( 'NONE', #7391, #18208 ) ;
#8861 = ORIENTED_EDGE ( 'NONE', *, *, #14831, .F. ) ;
#8862 = FACE_OUTER_BOUND ( 'NONE', #8993, .T. ) ;
#8863 = EDGE_LOOP ( 'NONE', ( #19279, #17987, #2133, #19186 ) ) ;
#8864 = CARTESIAN_POINT ( 'NONE',  ( 3.175194142252359963, -39.74634503291702003, -9.000000000000000000 ) ) ;
#8865 = CARTESIAN_POINT ( 'NONE',  ( 2.449293598294706513E-15, -20.00000000000000000, -9.000000000000000000 ) ) ;
#8866 = CARTESIAN_POINT ( 'NONE',  ( 53.54508667620428497, 60.29948385550240175, 4.840751629271157874 ) ) ;
#8867 = LINE ( 'NONE', #6123, #10086 ) ;
#8868 = DIRECTION ( 'NONE',  ( 0.000000000000000000, 0.000000000000000000, -1.000000000000000000 ) ) ;
#8869 = CARTESIAN_POINT ( 'NONE',  ( 57.61547081786810764, 52.90051614449766504, -2.450534656007114176 ) ) ;
#8870 = CARTESIAN_POINT ( 'NONE',  ( 46.49166364869456913, 48.30051614449765651, -4.867452303228181343 ) ) ;
#8871 = CARTESIAN_POINT ( 'NONE',  ( 0.000000000000000000, 4.041451884327382338, 0.000000000000000000 ) ) ;
#8872 = PLANE ( 'NONE',  #8761 ) ;
#8873 = ORIENTED_EDGE ( 'NONE', *, *, #7704, .F. ) ;
#8874 = ORIENTED_EDGE ( 'NONE', *, *, #9965, .F. ) ;
#8875 = CARTESIAN_POINT ( 'NONE',  ( -2.344047193898593395, -3.265465875126480455, -1.054683074273691752E-14 ) ) ;
#8876 = VERTEX_POINT ( 'NONE', #4933 ) ;
#8877 = APPLICATION_CONTEXT ( 'automotive_design' ) ;
#8878 = CARTESIAN_POINT ( 'NONE',  ( -154.9999999999999716, -14.99999999999999645, -15.00000000000000000 ) ) ;
#8879 = EDGE_LOOP ( 'NONE', ( #4070, #12391, #12227, #6893 ) ) ;
#8880 = DIRECTION ( 'NONE',  ( 0.000000000000000000, 0.000000000000000000, 1.000000000000000000 ) ) ;
#8881 = CARTESIAN_POINT ( 'NONE',  ( 43.33558569842703179, 47.09948385550240602, -2.141517661632099223 ) ) ;
#8882 = VECTOR ( 'NONE', #7778, 1000.000000000000000 ) ;
#8883 = ORIENTED_EDGE ( 'NONE', *, *, #7359, .T. ) ;
#8884 = DIRECTION ( 'NONE',  ( 2.775466039758894710E-17, 2.253973589064049552E-19, -1.000000000000000000 ) ) ;
#8885 = ORIENTED_EDGE ( 'NONE', *, *, #6804, .T. ) ;
#8886 = AXIS2_PLACEMENT_3D ( 'NONE', #5862, #11830, #17833 ) ;
#8887 = DIRECTION ( 'NONE',  ( 1.000000000000000000, 0.000000000000000000, 0.000000000000000000 ) ) ;
#8888 = CARTESIAN_POINT ( 'NONE',  ( 54.09612160359786515, 59.69948385550240033, -5.676469297603166098 ) ) ;
#8889 = FACE_OUTER_BOUND ( 'NONE', #3907, .T. ) ;
#8890 = CARTESIAN_POINT ( 'NONE',  ( 47.70284917648459100, 53.60051614449765367, 6.992620115222796251 ) ) ;
#8891 = LINE ( 'NONE', #14674, #14877 ) ;
#8892 = EDGE_CURVE ( 'NONE', #7505, #7366, #3606, .T. ) ;
#8893 = SURFACE_STYLE_USAGE ( .BOTH. , #1162 ) ;
#8894 = FACE_OUTER_BOUND ( 'NONE', #17719, .T. ) ;
#8895 = ORIENTED_EDGE ( 'NONE', *, *, #4237, .T. ) ;
#8896 = VECTOR ( 'NONE', #2396, 1000.000000000000227 ) ;
#8897 = ORIENTED_EDGE ( 'NONE', *, *, #11770, .T. ) ;
#8898 = ORIENTED_EDGE ( 'NONE', *, *, #670, .T. ) ;
#8899 = DIRECTION ( 'NONE',  ( -1.000000000000000000, 0.000000000000000000, 0.000000000000000000 ) ) ;
#8900 =( LENGTH_UNIT ( ) NAMED_UNIT ( * ) SI_UNIT ( .MILLI., .METRE. ) );
#8901 = CARTESIAN_POINT ( 'NONE',  ( 49.97728705011486738, 63.49948385550241170, -8.000000000000001776 ) ) ;
#8902 = LINE ( 'NONE', #5975, #4656 ) ;
#8903 = ORIENTED_EDGE ( 'NONE', *, *, #7237, .F. ) ;
#8904 = CARTESIAN_POINT ( 'NONE',  ( 6.518095160331716542, 5.866179305615093043, 1.445124054326800857E-15 ) ) ;
#8905 = ADVANCED_FACE ( 'NONE', ( #15816 ), #14557, .T. ) ;
#8906 = EDGE_LOOP ( 'NONE', ( #18500, #5619, #1855, #5134 ) ) ;
#8907 = CARTESIAN_POINT ( 'NONE',  ( 54.09612160359792199, 59.30051614449766362, 5.676469297603124353 ) ) ;
#8908 = ORIENTED_EDGE ( 'NONE', *, *, #6096, .F. ) ;
#8909 = CARTESIAN_POINT ( 'NONE',  ( 1.144235203016666258, 3.958177651039090250, -0.09382832055445661235 ) ) ;
#8910 = PRODUCT_DEFINITION_CONTEXT ( 'detailed design', #10022, 'design' ) ;
#8911 = FACE_OUTER_BOUND ( 'NONE', #13407, .T. ) ;
#8912 = AXIS2_PLACEMENT_3D ( 'NONE', #6360, #4806, #4985 ) ;
#8913 = CARTESIAN_POINT ( 'NONE',  ( 43.69122665457040000, 46.00051614449764514, -0.02388180880515696977 ) ) ;
#8914 = CARTESIAN_POINT ( 'NONE',  ( -0.1481481481481481122, -4.797713218419819903, -1.000000000000000000 ) ) ;
#8915 = EDGE_CURVE ( 'NONE', #13221, #17668, #15280, .T. ) ;
#8916 = FILL_AREA_STYLE_COLOUR ( '', #13652 ) ;
#8917 = ADVANCED_FACE ( 'NONE', ( #14758 ), #2917, .F. ) ;
#8918 = CARTESIAN_POINT ( 'NONE',  ( 55.11794222512601493, 56.19948385550240744, 3.688883143319541702 ) ) ;
#8919 = CARTESIAN_POINT ( 'NONE',  ( -54.99999999999996447, -14.99999999999998579, 15.00000000000000178 ) ) ;
#8920 = CARTESIAN_POINT ( 'NONE',  ( 52.29715082351547295, 54.39948385550239607, 6.992620115222774047 ) ) ;
#8921 = CARTESIAN_POINT ( 'NONE',  ( 54.68390685589039890, 51.30051614449765651, 6.485486291978072693 ) ) ;
#8922 = CARTESIAN_POINT ( 'NONE',  ( 0.4465819873852049926, -5.773502691896263528, -3.127607256515468906E-17 ) ) ;
#8923 = CARTESIAN_POINT ( 'NONE',  ( 4.158806965674307854, 4.075748668183981849, 0.05940377217583739378 ) ) ;
#8924 = DIRECTION ( 'NONE',  ( 1.000000000000000000, 0.000000000000000000, 0.000000000000000000 ) ) ;
#8925 = ADVANCED_FACE ( 'NONE', ( #11714 ), #7315, .F. ) ;
#8926 = PRODUCT_CONTEXT ( 'NONE', #2888, 'mechanical' ) ;
#8927 = CIRCLE ( 'NONE', #3295, 3.799999999999993605 ) ;
#8928 = EDGE_CURVE ( 'NONE', #14856, #8706, #7671, .T. ) ;
#8929 = ORIENTED_EDGE ( 'NONE', *, *, #16111, .F. ) ;
#8930 = PLANE ( 'NONE',  #6743 ) ;
#8931 = EDGE_CURVE ( 'NONE', #11964, #12225, #10531, .T. ) ;
#8932 = CARTESIAN_POINT ( 'NONE',  ( 1.149999999999998135, 0.000000000000000000, -4.100000000000000533 ) ) ;
#8933 = CIRCLE ( 'NONE', #3615, 20.00000000000000000 ) ;
#8934 = CARTESIAN_POINT ( 'NONE',  ( 0.000000000000000000, -3.031088913245531202, 1.750000000000006439 ) ) ;
#8935 = DIRECTION ( 'NONE',  ( -0.000000000000000000, -0.000000000000000000, 1.000000000000000000 ) ) ;
#8936 = LINE ( 'NONE', #10302, #18314 ) ;
#8937 = FACE_OUTER_BOUND ( 'NONE', #15092, .T. ) ;
#8938 = CARTESIAN_POINT ( 'NONE',  ( 43.33558569842703179, 61.09948385550240602, -2.141517661632099223 ) ) ;
#8939 = LINE ( 'NONE', #6104, #1703 ) ;
#8940 = CARTESIAN_POINT ( 'NONE',  ( 50.02271294988513972, 50.49948385550239749, 8.000000000000001776 ) ) ;
#8941 = CARTESIAN_POINT ( 'NONE',  ( 1.925929944387235853E-31, 15.00000000000001599, 9.000000000000000000 ) ) ;
#8942 = CARTESIAN_POINT ( 'NONE',  ( 43.33558569842706021, 53.90051614449765793, 2.141517661632167169 ) ) ;
#8943 = DIRECTION ( 'NONE',  ( -0.000000000000000000, 1.000000000000000000, -0.000000000000000000 ) ) ;
#8944 = VERTEX_POINT ( 'NONE', #14658 ) ;
#8945 = ORIENTED_EDGE ( 'NONE', *, *, #12511, .T. ) ;
#8946 = ORIENTED_EDGE ( 'NONE', *, *, #14890, .F. ) ;
#8947 = AXIS2_PLACEMENT_3D ( 'NONE', #18348, #11054, #12338 ) ;
#8948 = DIRECTION ( 'NONE',  ( 0.000000000000000000, 0.000000000000000000, -1.000000000000000000 ) ) ;
#8949 = VERTEX_POINT ( 'NONE', #17721 ) ;
#8950 = CYLINDRICAL_SURFACE ( 'NONE', #9713, 5.000000000000000888 ) ;
#8951 = EDGE_CURVE ( 'NONE', #4855, #15708, #1437, .T. ) ;
#8952 = ORIENTED_EDGE ( 'NONE', *, *, #669, .T. ) ;
#8953 = DIRECTION ( 'NONE',  ( -1.000000000000000000, 0.000000000000000000, 0.000000000000000000 ) ) ;
#8954 = ORIENTED_EDGE ( 'NONE', *, *, #6521, .T. ) ;
#8955 = CARTESIAN_POINT ( 'NONE',  ( -0.2000000000000000111, -6.997142273814360713, -0.8000000000000000444 ) ) ;
#8956 = CARTESIAN_POINT ( 'NONE',  ( 30.00000000000000355, 0.000000000000000000, -10.00000000000000000 ) ) ;
#8957 = EDGE_CURVE ( 'NONE', #15433, #11712, #1725, .T. ) ;
#8958 = CARTESIAN_POINT ( 'NONE',  ( 55.69932041026404335, 55.89948385550241028, -1.875703265242203432 ) ) ;
#8959 = DIRECTION ( 'NONE',  ( -0.9999670257950099561, -0.008120795692649453515, 0.000000000000000000 ) ) ;
#8960 = SURFACE_STYLE_USAGE ( .BOTH. , #1911 ) ;
#8961 = CARTESIAN_POINT ( 'NONE',  ( 42.39856655714564226, 56.10051614449766078, -2.493737253992044156 ) ) ;
#8962 = CARTESIAN_POINT ( 'NONE',  ( 48.02776887271750184, 55.60051614449765367, 5.992620115222795363 ) ) ;
#8963 = CARTESIAN_POINT ( 'NONE',  ( 14.17539641854931176, -34.10879641843979471, 9.000000000000000000 ) ) ;
#8964 = CARTESIAN_POINT ( 'NONE',  ( -4.799999999999999822, 5.878304635907294211E-16, -1.000000000000000000 ) ) ;
#8965 = ORIENTED_EDGE ( 'NONE', *, *, #17186, .F. ) ;
#8966 = B_SPLINE_CURVE_WITH_KNOTS ( 'NONE', 3,
 ( #4335, #4537, #10595, #16597, #3171 ),
 .UNSPECIFIED., .F., .F.,
 ( 4, 1, 4 ),
 ( 0.000000000000000000, 0.002886751345948122913, 0.005773502691896245827 ),
 .UNSPECIFIED. ) ;
#8967 = B_SPLINE_CURVE_WITH_KNOTS ( 'NONE', 3,
 ( #5503, #16402, #11477, #8934 ),
 .UNSPECIFIED., .F., .F.,
 ( 4, 4 ),
 ( 2.380739282168708963E-07, 0.002044882221487539717 ),
 .UNSPECIFIED. ) ;
#8968 = ORIENTED_EDGE ( 'NONE', *, *, #5127, .F. ) ;
#8969 = CARTESIAN_POINT ( 'NONE',  ( 2.000000000000000000, 0.000000000000000000, 0.000000000000000000 ) ) ;
#8970 = CIRCLE ( 'NONE', #17751, 1.610000000000000098 ) ;
#8971 = ORIENTED_EDGE ( 'NONE', *, *, #8308, .F. ) ;
#8972 = CARTESIAN_POINT ( 'NONE',  ( 54.13287192849676188, 64.29948385550241596, 5.649768623646098220 ) ) ;
#8973 = CARTESIAN_POINT ( 'NONE',  ( -14.00000000000000000, 15.00000000000001599, -9.000000000000000000 ) ) ;
#8974 = VERTEX_POINT ( 'NONE', #8148 ) ;
#8975 = FACE_OUTER_BOUND ( 'NONE', #14631, .T. ) ;
#8976 = CARTESIAN_POINT ( 'NONE',  ( 52.29715082351547295, 46.39948385550240317, 6.992620115222774047 ) ) ;
#8977 = MANIFOLD_SOLID_BREP ( 'Hex', #10536 ) ;
#8978 = ORIENTED_EDGE ( 'NONE', *, *, #7832, .T. ) ;
#8979 = FACE_OUTER_BOUND ( 'NONE', #13523, .T. ) ;
#8980 = ORIENTED_EDGE ( 'NONE', *, *, #9621, .F. ) ;
#8981 = CARTESIAN_POINT ( 'NONE',  ( 45.31609314410960820, 64.30051614449766362, -6.485486291978072693 ) ) ;
#8982 = LINE ( 'NONE', #9079, #15101 ) ;
#8983 = CIRCLE ( 'NONE', #13362, 2.149999999999999023 ) ;
#8984 = CARTESIAN_POINT ( 'NONE',  ( 44.05948171654949874, 60.79948385550240886, 4.345558710429105354 ) ) ;
#8985 = CARTESIAN_POINT ( 'NONE',  ( 0.000000000000000000, 0.000000000000000000, 0.000000000000000000 ) ) ;
#8986 = CARTESIAN_POINT ( 'NONE',  ( 42.63976443033212860, 52.00051614449766646, -0.02388180880514948964 ) ) ;
#8987 = DIRECTION ( 'NONE',  ( 0.000000000000000000, 0.000000000000000000, -1.000000000000000000 ) ) ;
#8988 = FILL_AREA_STYLE_COLOUR ( '', #15211 ) ;
#8989 = CARTESIAN_POINT ( 'NONE',  ( -4.000000000000000000, -2.472261339043343220, -3.687027428081192326 ) ) ;
#8990 = ORIENTED_EDGE ( 'NONE', *, *, #13409, .T. ) ;
#8991 = VERTEX_POINT ( 'NONE', #6681 ) ;
#8992 = AXIS2_PLACEMENT_3D ( 'NONE', #16112, #17490, #11385 ) ;
#8993 = EDGE_LOOP ( 'NONE', ( #10563, #14878, #17894, #2091 ) ) ;
#8994 = CARTESIAN_POINT ( 'NONE',  ( -54.99999999999996447, -22.99999999999998579, 10.00000000000000000 ) ) ;
#8995 =( NAMED_UNIT ( * ) PLANE_ANGLE_UNIT ( ) SI_UNIT ( $, .RADIAN. ) );
#8996 = CIRCLE ( 'NONE', #3069, 5.999999999999977796 ) ;
#8997 = CARTESIAN_POINT ( 'NONE',  ( 43.20883090819745576, 62.79948385550240175, 4.963592699179006473 ) ) ;
#8998 = PLANE ( 'NONE',  #12789 ) ;
#8999 = EDGE_LOOP ( 'NONE', ( #2140, #18326, #17694, #12584 ) ) ;
#9000 = CONICAL_SURFACE ( 'NONE', #551, 4.000000000000000000, 0.8911886515913786111 ) ;
#9001 = CARTESIAN_POINT ( 'NONE',  ( 2.499999999999999556, 0.000000000000000000, 3.469446951953614189E-15 ) ) ;
#9002 = ORIENTED_EDGE ( 'NONE', *, *, #16166, .F. ) ;
#9003 = CARTESIAN_POINT ( 'NONE',  ( 52.29715082351539479, 56.60051614449766078, -6.992620115222796251 ) ) ;
#9004 = ORIENTED_EDGE ( 'NONE', *, *, #14050, .F. ) ;
#9005 = CARTESIAN_POINT ( 'NONE',  ( 6.534838248920900483, -5.903531555104836848, 4.671345613696493211E-16 ) ) ;
#9006 = CYLINDRICAL_SURFACE ( 'NONE', #4276, 2.000000000000001776 ) ;
#9007 = AXIS2_PLACEMENT_3D ( 'NONE', #6787, #12771, #3855 ) ;
#9008 = CARTESIAN_POINT ( 'NONE',  ( 44.91013252490150620, 56.20051614449766220, -3.727524721679154940 ) ) ;
#9009 = CARTESIAN_POINT ( 'NONE',  ( -7.092489211676000613E-16, -4.452621892014641425, -2.287832656137186671 ) ) ;
#9010 = DIRECTION ( 'NONE',  ( -0.000000000000000000, -0.000000000000000000, 1.000000000000000000 ) ) ;
#9011 = CARTESIAN_POINT ( 'NONE',  ( 53.50833635130540955, 57.69948385550241454, -4.867452303228209765 ) ) ;
#9012 = FACE_OUTER_BOUND ( 'NONE', #936, .T. ) ;
#9013 = CARTESIAN_POINT ( 'NONE',  ( 47.42335538002180328, 56.40051614449765793, -8.007379884777206414 ) ) ;
#9014 = DIRECTION ( 'NONE',  ( 1.000000000000000000, 0.000000000000000000, 0.000000000000000000 ) ) ;
#9015 = CARTESIAN_POINT ( 'NONE',  ( -4.198928548860774157, 0.8158838809860065044, -3.526471437616918170 ) ) ;
#9016 = CARTESIAN_POINT ( 'NONE',  ( -4.688877333428352223, -21.02685410450703074, 9.999999999999998224 ) ) ;
#9017 = SHAPE_DEFINITION_REPRESENTATION ( #19343, #8665 ) ;
#9018 = ORIENTED_EDGE ( 'NONE', *, *, #6507, .F. ) ;
#9019 = CARTESIAN_POINT ( 'NONE',  ( 0.000000000000000000, 0.000000000000000000, 0.000000000000000000 ) ) ;
#9020 = VECTOR ( 'NONE', #19333, 1000.000000000000000 ) ;
#9021 = EDGE_CURVE ( 'NONE', #6185, #5879, #12681, .T. ) ;
#9022 = CIRCLE ( 'NONE', #5275, 4.800000000000000711 ) ;
#9023 = CARTESIAN_POINT ( 'NONE',  ( 2.482347295856823136E-15, -20.00000000000000000, -8.999999999999996447 ) ) ;
#9024 = EDGE_CURVE ( 'NONE', #7144, #10315, #9220, .T. ) ;
#9025 = CARTESIAN_POINT ( 'NONE',  ( 50.00000000000000000, 40.00000000000000000, 4.000000000000003553 ) ) ;
#9026 = PRESENTATION_LAYER_ASSIGNMENT (  '', '', ( #2780 ) ) ;
#9027 = CARTESIAN_POINT ( 'NONE',  ( 62.50000000000000000, 32.50000000000001421, 15.00000000000000000 ) ) ;
#9028 = CARTESIAN_POINT ( 'NONE',  ( 0.000000000000000000, 0.000000000000000000, 0.000000000000000000 ) ) ;
#9029 = EDGE_CURVE ( 'NONE', #9930, #5544, #14868, .T. ) ;
#9030 = EDGE_CURVE ( 'NONE', #5728, #16469, #3847, .T. ) ;
#9031 = CARTESIAN_POINT ( 'NONE',  ( 32.49999999999998579, 5.000000000000018652, 5.000000000000003553 ) ) ;
#9032 = CARTESIAN_POINT ( 'NONE',  ( 42.63976443033212860, 56.99948385550241170, 0.02388180880522514787 ) ) ;
#9033 = CARTESIAN_POINT ( 'NONE',  ( 0.000000000000000000, 0.000000000000000000, 0.000000000000000000 ) ) ;
#9034 = CARTESIAN_POINT ( 'NONE',  ( 58.41169779390614281, 53.99948385550241170, -0.02388180880523160798 ) ) ;
#9035 = DIRECTION ( 'NONE',  ( 1.000000000000000000, 0.000000000000000000, 0.000000000000000000 ) ) ;
#9036 = CARTESIAN_POINT ( 'NONE',  ( 43.33558569842706021, 51.90051614449765793, 2.141517661632167169 ) ) ;
#9037 = CIRCLE ( 'NONE', #6528, 0.1000000000000011297 ) ;
#9038 = ADVANCED_FACE ( 'NONE', ( #11178 ), #2083, .F. ) ;
#9039 = DIRECTION ( 'NONE',  ( -0.000000000000000000, -0.000000000000000000, 1.000000000000000000 ) ) ;
#9040 = VERTEX_POINT ( 'NONE', #14218 ) ;
#9041 = FILL_AREA_STYLE_COLOUR ( '', #17203 ) ;
#9042 = VERTEX_POINT ( 'NONE', #8045 ) ;
#9043 = ADVANCED_FACE ( 'NONE', ( #6231 ), #607, .T. ) ;
#9044 = ADVANCED_FACE ( 'NONE', ( #17185 ), #17383, .F. ) ;
#9045 = CARTESIAN_POINT ( 'NONE',  ( 6.420058897733097680, 2.891482565094591006, -5.008194711943424693 ) ) ;
#9046 = ORIENTED_EDGE ( 'NONE', *, *, #5311, .T. ) ;
#9047 = CARTESIAN_POINT ( 'NONE',  ( 6.196878017913830305, 5.292377467571572680, -0.8333333333333333703 ) ) ;
#9048 = VECTOR ( 'NONE', #7389, 1000.000000000000000 ) ;
#9049 = VECTOR ( 'NONE', #3108, 1000.000000000000000 ) ;
#9050 = PLANE ( 'NONE',  #16644 ) ;
#9051 = DIRECTION ( 'NONE',  ( 1.000000000000000000, 0.000000000000000000, 0.000000000000000000 ) ) ;
#9052 = EDGE_LOOP ( 'NONE', ( #16319, #15565, #16298, #17823 ) ) ;
#9053 = DIRECTION ( 'NONE',  ( -1.000000000000000000, 0.000000000000000000, 0.000000000000000000 ) ) ;
#9054 = CARTESIAN_POINT ( 'NONE',  ( 1.925929944387235853E-31, 15.00000000000001599, 9.000000000000000000 ) ) ;
#9055 = CARTESIAN_POINT ( 'NONE',  ( 43.69122665457040000, 54.99948385550239749, 0.02388180880521036456 ) ) ;
#9056 = FACE_OUTER_BOUND ( 'NONE', #13804, .T. ) ;
#9057 = CARTESIAN_POINT ( 'NONE',  ( 43.20883090819742023, 52.20051614449766220, -4.963592699178938972 ) ) ;
#9058 = CARTESIAN_POINT ( 'NONE',  ( 55.71335778527780036, 54.90051614449765793, -1.832500667257213056 ) ) ;
#9059 = CARTESIAN_POINT ( 'NONE',  ( -20.63749999999999574, 6.827405905246494173E-16, 5.575000000000000178 ) ) ;
#9060 = CARTESIAN_POINT ( 'NONE',  ( -7.211304515372694901, -1.345319965580611843, 9.000000000000000000 ) ) ;
#9061 = CIRCLE ( 'NONE', #17227, 20.00000000000000000 ) ;
#9062 = VERTEX_POINT ( 'NONE', #15605 ) ;
#9063 = ORIENTED_EDGE ( 'NONE', *, *, #9739, .F. ) ;
#9064 = LINE ( 'NONE', #531, #7807 ) ;
#9065 = ORIENTED_EDGE ( 'NONE', *, *, #1976, .F. ) ;
#9066 = CARTESIAN_POINT ( 'NONE',  ( 55.96859303347804371, 62.19948385550240744, 4.306917132069425946 ) ) ;
#9067 = CYLINDRICAL_SURFACE ( 'NONE', #7176, 2.149999999999999023 ) ;
#9068 = AXIS2_PLACEMENT_3D ( 'NONE', #2778, #7371, #19065 ) ;
#9069 = EDGE_CURVE ( 'NONE', #2467, #2682, #9710, .T. ) ;
#9070 = VERTEX_POINT ( 'NONE', #12461 ) ;
#9071 = CARTESIAN_POINT ( 'NONE',  ( 32.00000000000000000, -3.000000000000000000, 6.000000000000001776 ) ) ;
#9072 = CARTESIAN_POINT ( 'NONE',  ( 2.500000000000000444, 0.000000000000000000, -5.000000000000000888 ) ) ;
#9073 = EDGE_CURVE ( 'NONE', #15947, #18931, #16143, .T. ) ;
#9074 = ORIENTED_EDGE ( 'NONE', *, *, #6378, .F. ) ;
#9075 = CARTESIAN_POINT ( 'NONE',  ( 0.000000000000000000, 0.000000000000000000, 0.000000000000000000 ) ) ;
#9076 = ORIENTED_EDGE ( 'NONE', *, *, #11794, .T. ) ;
#9077 = CARTESIAN_POINT ( 'NONE',  ( 41.58830220609386430, 46.99948385550239749, 0.02388180880523263147 ) ) ;
#9078 = VECTOR ( 'NONE', #16062, 1000.000000000000000 ) ;
#9079 = CARTESIAN_POINT ( 'NONE',  ( -62.49999999999997158, 45.00000000000001421, -9.999999999999998224 ) ) ;
#9080 = CARTESIAN_POINT ( 'NONE',  ( 55.96859303347804371, 60.19948385550240744, 4.306917132069425946 ) ) ;
#9081 = DIRECTION ( 'NONE',  ( 0.000000000000000000, 0.000000000000000000, -1.000000000000000000 ) ) ;
#9082 = CARTESIAN_POINT ( 'NONE',  ( 4.000000000000000000, 0.000000000000000000, 0.000000000000000000 ) ) ;
#9083 = VECTOR ( 'NONE', #17375, 999.9999999999998863 ) ;
#9084 = VECTOR ( 'NONE', #9455, 1000.000000000000000 ) ;
#9085 = CARTESIAN_POINT ( 'NONE',  ( 55.94051828345053679, 51.20051614449766220, 4.345558710429044069 ) ) ;
#9086 = CARTESIAN_POINT ( 'NONE',  ( 2.500000000000000888, 3.061616997868384127E-16, -4.974599999999998801 ) ) ;
#9087 = DIRECTION ( 'NONE',  ( 1.000000000000000000, 0.000000000000000000, -0.000000000000000000 ) ) ;
#9088 = AXIS2_PLACEMENT_3D ( 'NONE', #17499, #14445, #17306 ) ;
#9089 = DIRECTION ( 'NONE',  ( 0.000000000000000000, 0.000000000000000000, -1.000000000000000000 ) ) ;
#9090 = ORIENTED_EDGE ( 'NONE', *, *, #3635, .T. ) ;
#9091 = EDGE_CURVE ( 'NONE', #6947, #14650, #2386, .T. ) ;
#9092 = VERTEX_POINT ( 'NONE', #900 ) ;
#9093 = ORIENTED_EDGE ( 'NONE', *, *, #17571, .F. ) ;
#9094 = DIRECTION ( 'NONE',  ( -0.000000000000000000, -0.000000000000000000, -1.000000000000000000 ) ) ;
#9095 =( NAMED_UNIT ( * ) SI_UNIT ( $, .STERADIAN. ) SOLID_ANGLE_UNIT ( ) );
#9096 = VECTOR ( 'NONE', #17659, 1000.000000000000000 ) ;
#9097 = EDGE_CURVE ( 'NONE', #3087, #4800, #16757, .T. ) ;
#9098 = CARTESIAN_POINT ( 'NONE',  ( 57.36023556966787851, 47.99948385550239038, -0.02388180880522424582 ) ) ;
#9099 = CARTESIAN_POINT ( 'NONE',  ( 62.49999999999998579, 32.50000000000001421, 15.00000000000000000 ) ) ;
#9100 = VECTOR ( 'NONE', #12248, 1000.000000000000000 ) ;
#9101 = CIRCLE ( 'NONE', #3481, 1.000000000000000888 ) ;
#9102 = ORIENTED_EDGE ( 'NONE', *, *, #504, .T. ) ;
#9103 = DIRECTION ( 'NONE',  ( -1.000000000000000000, 0.000000000000000000, 0.000000000000000000 ) ) ;
#9104 = CIRCLE ( 'NONE', #3469, 2.649999999999988365 ) ;
#9105 = ORIENTED_EDGE ( 'NONE', *, *, #10704, .T. ) ;
#9106 = CARTESIAN_POINT ( 'NONE',  ( 52.25172492374528588, 59.40051614449765793, 7.007379884777204637 ) ) ;
#9107 = ORIENTED_EDGE ( 'NONE', *, *, #15447, .F. ) ;
#9108 = DIRECTION ( 'NONE',  ( -1.000000000000000000, -0.000000000000000000, -0.000000000000000000 ) ) ;
#9109 = UNCERTAINTY_MEASURE_WITH_UNIT (LENGTH_MEASURE( 1.000000000000000082E-05 ), #18621, 'distance_accuracy_value', 'NONE');
#9110 = DIRECTION ( 'NONE',  ( 1.000000000000000000, 0.000000000000000000, -0.000000000000000000 ) ) ;
#9112 = AXIS2_PLACEMENT_3D ( 'NONE', #6079, #12624, #12333 ) ;
#9111 = CARTESIAN_POINT ( 'NONE',  ( 46.49166364869456913, 54.30051614449765651, -4.867452303228181343 ) ) ;
#9113 = DIRECTION ( 'NONE',  ( 1.000000000000000000, 0.000000000000000000, -0.000000000000000000 ) ) ;
#9114 = CARTESIAN_POINT ( 'NONE',  ( -19.89043790736547379, -17.90943073464699609, 9.000000000000000000 ) ) ;
#9115 = CARTESIAN_POINT ( 'NONE',  ( 55.08986747509847248, 57.79948385550240175, -3.727524721679197572 ) ) ;
#9116 = CARTESIAN_POINT ( 'NONE',  ( 2.807080416178989513, -3.225969019225150003, -3.502507215260505014 ) ) ;
#9117 = TOROIDAL_SURFACE ( 'NONE', #18849, 5.384454397937118664, 0.5155456020628804703 ) ;
#9118 = CARTESIAN_POINT ( 'NONE',  ( 50.02271294988505446, 52.50051614449766646, -8.000000000000001776 ) ) ;
#9119 = CARTESIAN_POINT ( 'NONE',  ( 6.095473853218515536, -4.853892138987517590, 1.592812200814445633 ) ) ;
#9120 = CARTESIAN_POINT ( 'NONE',  ( 3.972066048304756514, 2.740530939476224059, -2.384802634787894338 ) ) ;
#9121 = EDGE_LOOP ( 'NONE', ( #13566, #5519 ) ) ;
#9122 = FACE_OUTER_BOUND ( 'NONE', #9740, .T. ) ;
#9123 =( LENGTH_UNIT ( ) NAMED_UNIT ( * ) SI_UNIT ( .MILLI., .METRE. ) );
#9124 = APPLICATION_PROTOCOL_DEFINITION ( 'draft international standard', 'automotive_design', 1998, #16692 ) ;
#9125 = ORIENTED_EDGE ( 'NONE', *, *, #2957, .T. ) ;
#9126 = DIRECTION ( 'NONE',  ( 0.000000000000000000, 0.000000000000000000, 1.000000000000000000 ) ) ;
#9127 = DIRECTION ( 'NONE',  ( 0.000000000000000000, 0.000000000000000000, -1.000000000000000000 ) ) ;
#9128 = AXIS2_PLACEMENT_3D ( 'NONE', #15443, #16832, #15739 ) ;
#9129 = CIRCLE ( 'NONE', #11626, 6.080745460913608902 ) ;
#9130 = CARTESIAN_POINT ( 'NONE',  ( 54.09612160359786515, 63.69948385550240744, -5.676469297603166098 ) ) ;
#9131 = FACE_OUTER_BOUND ( 'NONE', #15370, .T. ) ;
#9132 = CARTESIAN_POINT ( 'NONE',  ( 2.449293598294706513E-15, -20.00000000000000000, -9.000000000000000000 ) ) ;
#9133 = DIRECTION ( 'NONE',  ( -1.000000000000000000, 0.000000000000000000, 0.000000000000000000 ) ) ;
#9134 = CARTESIAN_POINT ( 'NONE',  ( 47.74827507625478518, 58.59948385550238470, 7.007379884777227730 ) ) ;
#9135 = CARTESIAN_POINT ( 'NONE',  ( 1.250000000000000000, -6.429618962271402616, -1.000000000000000000 ) ) ;
#9136 = CARTESIAN_POINT ( 'NONE',  ( 47.42335538002188144, 56.59948385550239891, 8.007379884777233059 ) ) ;
#9137 = FACE_OUTER_BOUND ( 'NONE', #11308, .T. ) ;
#9138 = ADVANCED_FACE ( 'NONE', ( #15903, #4041 ), #14813, .T. ) ;
#9139 = CARTESIAN_POINT ( 'NONE',  ( 44.05948171654945611, 54.20051614449764799, -4.345558710429044069 ) ) ;
#9140 = DIRECTION ( 'NONE',  ( 0.000000000000000000, -0.8660254037844380415, -0.5000000000000009992 ) ) ;
#9141 = CIRCLE ( 'NONE', #11641, 2.000000000000000888 ) ;
#9142 = ORIENTED_EDGE ( 'NONE', *, *, #10943, .F. ) ;
#9143 = EDGE_CURVE ( 'NONE', #12835, #7144, #2775, .T. ) ;
#9144 = EDGE_CURVE ( 'NONE', #162, #18909, #8469, .T. ) ;
#9145 = CARTESIAN_POINT ( 'NONE',  ( 4.203833317240879275, 1.627343821129582979, -3.597273115243889929 ) ) ;
#9146 = ORIENTED_EDGE ( 'NONE', *, *, #2361, .F. ) ;
#9147 = DIRECTION ( 'NONE',  ( 1.000000000000000000, 0.000000000000000000, 0.000000000000000000 ) ) ;
#9148 = EDGE_CURVE ( 'NONE', #10775, #869, #6113, .T. ) ;
#9149 = CARTESIAN_POINT ( 'NONE',  ( 45.86712807150323812, 61.29948385550240886, -5.649768623646098220 ) ) ;
#9150 = EDGE_CURVE ( 'NONE', #4903, #17705, #10172, .T. ) ;
#9151 = VECTOR ( 'NONE', #12986, 1000.000000000000114 ) ;
#9152 = DIRECTION ( 'NONE',  ( 0.000000000000000000, 0.000000000000000000, 1.000000000000000000 ) ) ;
#9153 = ORIENTED_EDGE ( 'NONE', *, *, #1130, .F. ) ;
#9154 = DIRECTION ( 'NONE',  ( 0.000000000000000000, 0.000000000000000000, 1.000000000000000000 ) ) ;
#9155 = CARTESIAN_POINT ( 'NONE',  ( -9.999999999999998224, 15.00000000000001776, 15.00000000000000000 ) ) ;
#9156 = CARTESIAN_POINT ( 'NONE',  ( 46.49166364869460466, 56.69948385550240744, 4.867452303228209765 ) ) ;
#9157 = DIRECTION ( 'NONE',  ( 0.000000000000000000, 0.000000000000000000, 1.000000000000000000 ) ) ;
#9158 = FACE_OUTER_BOUND ( 'NONE', #12033, .T. ) ;
#9159 = CARTESIAN_POINT ( 'NONE',  ( 45.27934281921082516, 51.70051614449765509, 6.458785618021089192 ) ) ;
#9160 = EDGE_CURVE ( 'NONE', #18844, #3696, #4140, .T. ) ;
#9161 = CARTESIAN_POINT ( 'NONE',  ( 51.97223112728249816, 56.60051614449765367, -5.992620115222793586 ) ) ;
#9162 = EDGE_CURVE ( 'NONE', #17604, #15949, #8933, .T. ) ;
#9163 = CARTESIAN_POINT ( 'NONE',  ( 2.805705207896068476, -3.226868319750173075, -3.503898532754370354 ) ) ;
#9164 = CARTESIAN_POINT ( 'NONE',  ( 6.541171661047877173, -2.934678558896545386, -5.142480235691130552 ) ) ;
#9165 = ORIENTED_EDGE ( 'NONE', *, *, #9540, .F. ) ;
#9166 = VERTEX_POINT ( 'NONE', #8543 ) ;
#9167 = CARTESIAN_POINT ( 'NONE',  ( 6.092460485788117275, -1.005982284679170391, -5.000000000000000000 ) ) ;
#9168 = EDGE_LOOP ( 'NONE', ( #6025, #18597 ) ) ;
#9169 = ADVANCED_FACE ( 'NONE', ( #9902 ), #10038, .F. ) ;
#9170 = CARTESIAN_POINT ( 'NONE',  ( -154.9999999999999716, -14.99999999999999645, 15.00000000000000000 ) ) ;
#9171 = FACE_OUTER_BOUND ( 'NONE', #14834, .T. ) ;
#9172 = EDGE_CURVE ( 'NONE', #17851, #8408, #14421, .T. ) ;
#9173 = ORIENTED_EDGE ( 'NONE', *, *, #17812, .F. ) ;
#9174 = CARTESIAN_POINT ( 'NONE',  ( -7.499999999999998224, -20.00000000000000000, -20.00000000000000000 ) ) ;
#9175 = CARTESIAN_POINT ( 'NONE',  ( 47.74827507625477807, 50.59948385550239891, 7.007379884777229506 ) ) ;
#9176 = EDGE_CURVE ( 'NONE', #6411, #17357, #11749, .T. ) ;
#9177 = EDGE_LOOP ( 'NONE', ( #15272, #17047, #12482 ) ) ;
#9178 = DIRECTION ( 'NONE',  ( -0.9999670257950100671, -0.008120795692649436168, -2.775557561562891043E-17 ) ) ;
#9179 = ORIENTED_EDGE ( 'NONE', *, *, #7013, .T. ) ;
#9180 = CARTESIAN_POINT ( 'NONE',  ( 45.27934281921082516, 63.70051614449766930, 6.458785618021089192 ) ) ;
#9181 = CARTESIAN_POINT ( 'NONE',  ( 4.200000000000001954, 0.000000000000000000, 0.000000000000000000 ) ) ;
#9182 = CARTESIAN_POINT ( 'NONE',  ( 55.96859303347804371, 56.19948385550241454, 4.306917132069425946 ) ) ;
#9183 = DIRECTION ( 'NONE',  ( 1.000000000000000000, 0.000000000000000000, 0.000000000000000000 ) ) ;
#9184 = CARTESIAN_POINT ( 'NONE',  ( 45.90387839640208512, 56.30051614449765651, -5.676469297603124353 ) ) ;
#9185 = CARTESIAN_POINT ( 'NONE',  ( -149.0000000000000000, -14.99999999999999645, -6.499999999999999112 ) ) ;
#9186 = LINE ( 'NONE', #4963, #2863 ) ;
#9187 = VERTEX_POINT ( 'NONE', #19258 ) ;
#9188 = ORIENTED_EDGE ( 'NONE', *, *, #3415, .T. ) ;
#9189 = EDGE_LOOP ( 'NONE', ( #5748, #2366, #16817, #17111 ) ) ;
#9190 = CARTESIAN_POINT ( 'NONE',  ( -52.34999999999998010, -14.99999999999998579, -10.00000000000000178 ) ) ;
#9191 = CARTESIAN_POINT ( 'NONE',  ( 45.31609314410967926, 62.69948385550240744, 6.485486291978119766 ) ) ;
#9192 = ORIENTED_EDGE ( 'NONE', *, *, #18396, .F. ) ;
#9193 = CARTESIAN_POINT ( 'NONE',  ( 6.527192678185836705, 5.883244248022287515, -9.347031149521713219E-14 ) ) ;
#9194 = EDGE_LOOP ( 'NONE', ( #10264, #14096, #13904, #9259 ) ) ;
#9195 = CARTESIAN_POINT ( 'NONE',  ( 49.97728705011495265, 59.50051614449765935, 7.000000000000000888 ) ) ;
#9196 = ORIENTED_EDGE ( 'NONE', *, *, #4390, .T. ) ;
#9197 = EDGE_CURVE ( 'NONE', #6947, #12063, #183, .T. ) ;
#9198 = CARTESIAN_POINT ( 'NONE',  ( 6.244889965166096957, -4.918546365148221078, 1.691415889817839746 ) ) ;
#9199 = CARTESIAN_POINT ( 'NONE',  ( -1.000000000000000000, -6.008326913195983998, -0.8000000000000000444 ) ) ;
#9200 = CARTESIAN_POINT ( 'NONE',  ( 44.30067958973594955, 52.10051614449766788, -1.875703265242155693 ) ) ;
#9201 = CARTESIAN_POINT ( 'NONE',  ( 19.97007065299863271, -21.09374499507101319, -9.000000000000000000 ) ) ;
#9202 = EDGE_CURVE ( 'NONE', #5017, #10265, #10796, .T. ) ;
#9203 = VECTOR ( 'NONE', #12597, 1000.000000000000000 ) ;
#9204 = LINE ( 'NONE', #480, #7064 ) ;
#9205 = CARTESIAN_POINT ( 'NONE',  ( 56.30877334542961421, 59.99948385550241170, -0.02388180880520959434 ) ) ;
#9206 = DIRECTION ( 'NONE',  ( -0.000000000000000000, -0.000000000000000000, 1.000000000000000000 ) ) ;
#9207 = AXIS2_PLACEMENT_3D ( 'NONE', #721, #15426, #6788 ) ;
#9208 = CARTESIAN_POINT ( 'NONE',  ( 45.27934281921082516, 53.70051614449766220, 6.458785618021089192 ) ) ;
#9209 = DIRECTION ( 'NONE',  ( 9.858538378746663627E-23, -5.031452844637890958E-23, 1.000000000000000000 ) ) ;
#9210 = ORIENTED_EDGE ( 'NONE', *, *, #11304, .F. ) ;
#9211 = DIRECTION ( 'NONE',  ( -1.000000000000000000, 0.000000000000000000, 0.000000000000000000 ) ) ;
#9212 = CARTESIAN_POINT ( 'NONE',  ( 2.899426713160750069, -23.82535289025860337, -9.999999999999994671 ) ) ;
#9213 = SHAPE_DEFINITION_REPRESENTATION ( #17125, #9916 ) ;
#9214 = ORIENTED_EDGE ( 'NONE', *, *, #1986, .F. ) ;
#9215 = CARTESIAN_POINT ( 'NONE',  ( 0.000000000000000000, 40.00000000000001421, -9.999999999999998224 ) ) ;
#9216 = LINE ( 'NONE', #10590, #944 ) ;
#9217 = CARTESIAN_POINT ( 'NONE',  ( 44.05948171654949874, 62.79948385550240886, 4.345558710429104465 ) ) ;
#9218 = DIRECTION ( 'NONE',  ( -1.000000000000000000, -0.000000000000000000, -0.000000000000000000 ) ) ;
#9219 = FACE_BOUND ( 'NONE', #13463, .T. ) ;
#9220 = CIRCLE ( 'NONE', #4550, 5.000000000000000888 ) ;
#9221 = DIRECTION ( 'NONE',  ( -0.000000000000000000, -0.000000000000000000, 1.000000000000000000 ) ) ;
#9222 = CARTESIAN_POINT ( 'NONE',  ( 55.94051828345050836, 59.79948385550238754, -4.345558710429104465 ) ) ;
#9223 = CARTESIAN_POINT ( 'NONE',  ( -144.9999999999999716, -14.99999999999999467, 4.000000000000000000 ) ) ;
#9224 = CARTESIAN_POINT ( 'NONE',  ( 47.42335538002188144, 60.59948385550240602, 8.007379884777233059 ) ) ;
#9225 = CARTESIAN_POINT ( 'NONE',  ( 55.94051828345053679, 53.20051614449766220, 4.345558710429044069 ) ) ;
#9226 = CARTESIAN_POINT ( 'NONE',  ( 4.158233816354936607, -0.4370479853238358192, 9.000000000000000000 ) ) ;
#9227 = CIRCLE ( 'NONE', #1097, 2.000000000000001776 ) ;
#9228 =( NAMED_UNIT ( * ) PLANE_ANGLE_UNIT ( ) SI_UNIT ( $, .RADIAN. ) );
#9229 = VERTEX_POINT ( 'NONE', #7367 ) ;
#9230 = PRESENTATION_LAYER_ASSIGNMENT (  '', '', ( #4853 ) ) ;
#9231 = CARTESIAN_POINT ( 'NONE',  ( -14.17539641854910570, -34.10879641843999366, -9.000000000000000000 ) ) ;
#9232 = CARTESIAN_POINT ( 'NONE',  ( 47.70284917648459810, 45.60051614449765367, 6.992620115222797139 ) ) ;
#9233 = EDGE_CURVE ( 'NONE', #10636, #6141, #5488, .T. ) ;
#9234 = LINE ( 'NONE', #12283, #3447 ) ;
#9235 = DIRECTION ( 'NONE',  ( 0.000000000000000000, 0.000000000000000000, 1.000000000000000000 ) ) ;
#9236 = ORIENTED_EDGE ( 'NONE', *, *, #13243, .F. ) ;
#9237 = DIRECTION ( 'NONE',  ( 1.000000000000000000, 0.000000000000000000, 0.000000000000000000 ) ) ;
#9238 = CARTESIAN_POINT ( 'NONE',  ( 0.000000000000000000, 0.000000000000000000, 0.000000000000000000 ) ) ;
#9239 = CARTESIAN_POINT ( 'NONE',  ( 53.50833635130544508, 45.30051614449766362, 4.867452303228181343 ) ) ;
#9240 = CARTESIAN_POINT ( 'NONE',  ( 1.250000000000000666, 5.899999999999999467, 0.000000000000000000 ) ) ;
#9241 = LINE ( 'NONE', #18292, #12355 ) ;
#9242 = B_SPLINE_CURVE_WITH_KNOTS ( 'NONE', 3,
 ( #13750, #7871, #12370, #17293, #18669, #713, #9523, #807, #6587, #15512, #3556, #12666, #9908, #15810, #5211, #3653 ),
 .UNSPECIFIED., .F., .F.,
 ( 4, 3, 3, 3, 3, 4 ),
 ( 0.000000000000000000, 3.315506744709513341E-05, 6.608280158699547874E-05, 0.0001026520855291439131, 0.0001376952025664790686, 0.0001398064759190603148 ),
 .UNSPECIFIED. ) ;
#9243 = CARTESIAN_POINT ( 'NONE',  ( 47.42335538002180328, 50.40051614449766504, -8.007379884777206414 ) ) ;
#9244 = AXIS2_PLACEMENT_3D ( 'NONE', #1485, #6369, #3164 ) ;
#9245 = CARTESIAN_POINT ( 'NONE',  ( 55.69932041026405045, 55.10051614449765367, 1.875703265242156359 ) ) ;
#9246 = CARTESIAN_POINT ( 'NONE',  ( -4.197393957002303999, -0.8151795401431414234, -3.503767560748935139 ) ) ;
#9247 = CARTESIAN_POINT ( 'NONE',  ( 1.150000000000000577, 0.000000000000000000, -5.899999999999999467 ) ) ;
#9248 = ORIENTED_EDGE ( 'NONE', *, *, #9310, .F. ) ;
#9249 = EDGE_CURVE ( 'NONE', #6480, #8472, #794, .T. ) ;
#9250 = EDGE_LOOP ( 'NONE', ( #1830, #6501, #13589, #11948 ) ) ;
#9251 = CARTESIAN_POINT ( 'NONE',  ( 20.00000000000000000, -14.99999999999999289, -20.00000000000000000 ) ) ;
#9252 = ORIENTED_EDGE ( 'NONE', *, *, #1630, .F. ) ;
#9253 = DIRECTION ( 'NONE',  ( 0.9135454576426006446, 0.4067366430758008189, 0.000000000000000000 ) ) ;
#9254 = ORIENTED_EDGE ( 'NONE', *, *, #10706, .F. ) ;
#9255 = FACE_OUTER_BOUND ( 'NONE', #8182, .T. ) ;
#9256 = EDGE_CURVE ( 'NONE', #14216, #9274, #19269, .T. ) ;
#9257 = CARTESIAN_POINT ( 'NONE',  ( 44.05948171654949874, 52.79948385550240175, 4.345558710429104465 ) ) ;
#9258 = EDGE_CURVE ( 'NONE', #3492, #1565, #16590, .T. ) ;
#9259 = ORIENTED_EDGE ( 'NONE', *, *, #5677, .T. ) ;
#9260 = CARTESIAN_POINT ( 'NONE',  ( 2.449293598294706513E-15, -20.00000000000000000, 9.000000000000000000 ) ) ;
#9261 = ORIENTED_EDGE ( 'NONE', *, *, #1001, .T. ) ;
#9262 = CARTESIAN_POINT ( 'NONE',  ( 54.72065718078918906, 62.70051614449766220, -6.458785618021089192 ) ) ;
#9263 = CARTESIAN_POINT ( 'NONE',  ( 50.76502259767569569, 44.99999999999998579, -6.467049654501940914 ) ) ;
#9264 = EDGE_CURVE ( 'NONE', #7873, #10516, #6425, .T. ) ;
#9265 = CARTESIAN_POINT ( 'NONE',  ( 45.90387839640214196, 56.69948385550240744, 5.676469297603166098 ) ) ;
#9266 = CARTESIAN_POINT ( 'NONE',  ( -32.00000000000000000, -1.000000000000000000, -5.999999999999998224 ) ) ;
#9267 = AXIS2_PLACEMENT_3D ( 'NONE', #11852, #4421, #10183 ) ;
#9268 = CARTESIAN_POINT ( 'NONE',  ( 52.25172492374527877, 53.40051614449765793, 7.007379884777203749 ) ) ;
#9269 = ADVANCED_FACE ( 'NONE', ( #11969 ), #16495, .T. ) ;
#9270 = CARTESIAN_POINT ( 'NONE',  ( 6.196878017913830305, 1.924500897298746960, -4.999999999999999112 ) ) ;
#9271 = CARTESIAN_POINT ( 'NONE',  ( 43.33558569842703179, 53.09948385550240602, -2.141517661632099223 ) ) ;
#9272 = DIRECTION ( 'NONE',  ( 1.000000000000000000, 0.000000000000000000, 0.000000000000000000 ) ) ;
#9273 = AXIS2_PLACEMENT_3D ( 'NONE', #6120, #12187, #7678 ) ;
#9274 = VERTEX_POINT ( 'NONE', #1688 ) ;
#9275 = APPLICATION_CONTEXT ( 'automotive_design' ) ;
#9276 = EDGE_LOOP ( 'NONE', ( #19018, #5779, #4965, #14364 ) ) ;
#9277 = FACE_BOUND ( 'NONE', #4576, .T. ) ;
#9278 = PRESENTATION_STYLE_ASSIGNMENT (( #12322 ) ) ;
#9279 = CARTESIAN_POINT ( 'NONE',  ( 43.34962307344081012, 50.89948385550241028, 2.184720259617164650 ) ) ;
#9280 = FACE_BOUND ( 'NONE', #4063, .T. ) ;
#9281 = ORIENTED_EDGE ( 'NONE', *, *, #5191, .F. ) ;
#9282 = CYLINDRICAL_SURFACE ( 'NONE', #4578, 5.575000000000000178 ) ;
#9283 = EDGE_CURVE ( 'NONE', #8706, #12622, #4531, .T. ) ;
#9284 = VECTOR ( 'NONE', #3368, 1000.000000000000114 ) ;
#9285 = EDGE_CURVE ( 'NONE', #2433, #10922, #10688, .T. ) ;
#9286 = EDGE_LOOP ( 'NONE', ( #15930, #9459, #284, #8635, #2014, #5983, #11401, #16225 ) ) ;
#9287 = CARTESIAN_POINT ( 'NONE',  ( 57.36023556966787851, 57.00051614449766646, 0.02388180880515038476 ) ) ;
#9288 = EDGE_LOOP ( 'NONE', ( #7998, #19277, #5133, #3132 ) ) ;
#9289 = AXIS2_PLACEMENT_3D ( 'NONE', #11849, #5409, #17854 ) ;
#9290 = LINE ( 'NONE', #15279, #2246 ) ;
#9291 = PRODUCT_DEFINITION_CONTEXT ( 'detailed design', #18441, 'design' ) ;
#9292 = CYLINDRICAL_SURFACE ( 'NONE', #1482, 1.000000000000000888 ) ;
#9293 = CARTESIAN_POINT ( 'NONE',  ( 55.71335778527780036, 56.90051614449767214, -1.832500667257213056 ) ) ;
#9294 = FACE_OUTER_BOUND ( 'NONE', #4868, .T. ) ;
#9295 = CIRCLE ( 'NONE', #6175, 2.447112362156698140 ) ;
#9296 = CARTESIAN_POINT ( 'NONE',  ( 0.3117969352650131198, 2.419842229202155970, 4.999999999999999112 ) ) ;
#9297 = CARTESIAN_POINT ( 'NONE',  ( 53.54508667620424234, 44.70051614449765509, -4.840751629271188961 ) ) ;
#9298 = DIRECTION ( 'NONE',  ( 0.000000000000000000, 0.000000000000000000, -1.000000000000000000 ) ) ;
#9299 = CARTESIAN_POINT ( 'NONE',  ( 47.42335538002180328, 58.40051614449765793, -8.007379884777206414 ) ) ;
#9300 = AXIS2_PLACEMENT_3D ( 'NONE', #4046, #3949, #15908 ) ;
#9301 = EDGE_LOOP ( 'NONE', ( #15902, #4501, #6151, #1116 ) ) ;
#9302 = DIRECTION ( 'NONE',  ( 0.000000000000000000, 0.000000000000000000, 1.000000000000000000 ) ) ;
#9303 = AXIS2_PLACEMENT_3D ( 'NONE', #2650, #8514, #14484 ) ;
#9304 = VERTEX_POINT ( 'NONE', #7561 ) ;
#9305 = APPLICATION_PROTOCOL_DEFINITION ( 'draft international standard', 'automotive_design', 1998, #13036 ) ;
#9306 = ORIENTED_EDGE ( 'NONE', *, *, #16359, .T. ) ;
#9307 = DIRECTION ( 'NONE',  ( 0.1045284632676494602, 0.9945218953682738450, 0.000000000000000000 ) ) ;
#9308 = EDGE_CURVE ( 'NONE', #2369, #828, #16466, .T. ) ;
#9309 = DIRECTION ( 'NONE',  ( 0.9135454576426060846, -0.4067366430757887730, 0.000000000000000000 ) ) ;
#9310 = EDGE_CURVE ( 'NONE', #16610, #12297, #1752, .T. ) ;
#9311 = AXIS2_PLACEMENT_3D ( 'NONE', #12276, #13920, #506 ) ;
#9312 = EDGE_CURVE ( 'NONE', #2433, #9835, #6189, .T. ) ;
#9313 = DIRECTION ( 'NONE',  ( 1.000000000000000000, 0.000000000000000000, 0.000000000000000000 ) ) ;
#9314 = CARTESIAN_POINT ( 'NONE',  ( -1.000000000000000000, -14.00000000000000000, -9.000000000000001776 ) ) ;
#9315 = PRESENTATION_LAYER_ASSIGNMENT (  '', '', ( #17791 ) ) ;
#9316 = DIRECTION ( 'NONE',  ( -1.000000000000000000, 0.000000000000000000, 0.000000000000000000 ) ) ;
#9317 = DIRECTION ( 'NONE',  ( 0.000000000000000000, 0.000000000000000000, 1.000000000000000000 ) ) ;
#9318 = CARTESIAN_POINT ( 'NONE',  ( 49.97728705011488870, 47.49948385550240459, -6.000000000000000888 ) ) ;
#9319 = DIRECTION ( 'NONE',  ( 0.000000000000000000, 0.000000000000000000, 1.000000000000000000 ) ) ;
#9320 = CARTESIAN_POINT ( 'NONE',  ( 57.60143344285433642, 61.89948385550241738, -2.493737253992118319 ) ) ;
#9321 = CARTESIAN_POINT ( 'NONE',  ( 47.70284917648459100, 51.60051614449765367, 6.992620115222796251 ) ) ;
#9322 = DIRECTION ( 'NONE',  ( 0.000000000000000000, 0.000000000000000000, -1.000000000000000000 ) ) ;
#9323 = FACE_OUTER_BOUND ( 'NONE', #14121, .T. ) ;
#9324 = EDGE_CURVE ( 'NONE', #18916, #206, #15825, .T. ) ;
#9325 = CIRCLE ( 'NONE', #9952, 2.649999999999985700 ) ;
#9326 = SURFACE_SIDE_STYLE ('',( #10794 ) ) ;
#9327 = ORIENTED_EDGE ( 'NONE', *, *, #1065, .F. ) ;
#9328 = EDGE_CURVE ( 'NONE', #17315, #18931, #7751, .T. ) ;
#9329 = CARTESIAN_POINT ( 'NONE',  ( 0.000000000000000000, 0.000000000000000000, -3.499999999999999556 ) ) ;
#9330 = CARTESIAN_POINT ( 'NONE',  ( 55.96859303347802239, 48.80051614449765651, -4.306917132069484566 ) ) ;
#9331 = CARTESIAN_POINT ( 'NONE',  ( 47.70284917648453415, 65.39948385550239607, -6.992620115222774047 ) ) ;
#9332 = DIRECTION ( 'NONE',  ( 0.000000000000000000, 0.000000000000000000, 1.000000000000000000 ) ) ;
#9333 = ORIENTED_EDGE ( 'NONE', *, *, #465, .T. ) ;
#9334 = CIRCLE ( 'NONE', #896, 2.649999999999989697 ) ;
#9335 = FACE_OUTER_BOUND ( 'NONE', #3766, .T. ) ;
#9336 = AXIS2_PLACEMENT_3D ( 'NONE', #4275, #19106, #10340 ) ;
#9337 = CARTESIAN_POINT ( 'NONE',  ( 51.92680522751233951, 63.59948385550239891, -6.007379884777223289 ) ) ;
#9338 = CARTESIAN_POINT ( 'NONE',  ( 15.51323935927282704, -32.62297130559633729, 9.000000000000000000 ) ) ;
#9339 = CARTESIAN_POINT ( 'NONE',  ( 47.37792948025170858, 61.60051614449765367, 7.992620115222797139 ) ) ;
#9340 = CARTESIAN_POINT ( 'NONE',  ( 46.45491332379576477, 57.70051614449766930, 4.840751629271188961 ) ) ;
#9341 = MECHANICAL_DESIGN_GEOMETRIC_PRESENTATION_REPRESENTATION (  '', ( #9970 ), #4665 ) ;
#9342 = CYLINDRICAL_SURFACE ( 'NONE', #14748, 5.400000000000000355 ) ;
#9343 = DIRECTION ( 'NONE',  ( 0.000000000000000000, 0.000000000000000000, 1.000000000000000000 ) ) ;
#9344 = ORIENTED_EDGE ( 'NONE', *, *, #6921, .F. ) ;
#9345 = VERTEX_POINT ( 'NONE', #3347 ) ;
#9346 = LINE ( 'NONE', #9251, #9981 ) ;
#9347 = ORIENTED_EDGE ( 'NONE', *, *, #12147, .F. ) ;
#9348 = AXIS2_PLACEMENT_3D ( 'NONE', #9858, #17239, #14562 ) ;
#9349 = AXIS2_PLACEMENT_3D ( 'NONE', #9735, #11106, #9635 ) ;
#9350 = CARTESIAN_POINT ( 'NONE',  ( 3.972709601346592123, -2.746729940827190575, 2.374099244652734697 ) ) ;
#9351 = VERTEX_POINT ( 'NONE', #16690 ) ;
#9352 = DIRECTION ( 'NONE',  ( 1.000000000000000000, 0.000000000000000000, 0.000000000000000000 ) ) ;
#9353 = CARTESIAN_POINT ( 'NONE',  ( 43.33558569842703179, 53.09948385550240602, -2.141517661632099223 ) ) ;
#9354 = ORIENTED_EDGE ( 'NONE', *, *, #465, .F. ) ;
#9355 = CARTESIAN_POINT ( 'NONE',  ( 1.734723475976807094E-15, 4.618802153517012954, -0.4999999999999995559 ) ) ;
#9356 = ORIENTED_EDGE ( 'NONE', *, *, #16139, .T. ) ;
#9357 = CARTESIAN_POINT ( 'NONE',  ( 54.68390685589033495, 47.69948385550240744, -6.485486291978119766 ) ) ;
#9358 = DIRECTION ( 'NONE',  ( 1.000000000000000000, 0.000000000000000000, 0.000000000000000000 ) ) ;
#9359 = CARTESIAN_POINT ( 'NONE',  ( 47.74827507625478518, 62.59948385550240602, 7.007379884777227730 ) ) ;
#9360 = CARTESIAN_POINT ( 'NONE',  ( 4.151274195509685683, 2.039912954708744230, -3.533232880573500267 ) ) ;
#9361 = CARTESIAN_POINT ( 'NONE',  ( 3.999999999999999112, -0.3979232138631231819, -5.929230630780099908E-17 ) ) ;
#9362 = CARTESIAN_POINT ( 'NONE',  ( 56.65037692655921120, 63.10051614449766078, 2.184720259617097593 ) ) ;
#9363 = AXIS2_PLACEMENT_3D ( 'NONE', #4279, #13198, #4380 ) ;
#9364 = AXIS2_PLACEMENT_3D ( 'NONE', #11153, #2062, #7932 ) ;
#9365 = CARTESIAN_POINT ( 'NONE',  ( -154.9999999999999716, -14.99999999999999645, 10.00000000000000000 ) ) ;
#9366 = CARTESIAN_POINT ( 'NONE',  ( 50.02271294988512551, 52.49948385550240459, 7.000000000000000888 ) ) ;
#9367 = DIRECTION ( 'NONE',  ( 0.000000000000000000, -0.000000000000000000, -1.000000000000000000 ) ) ;
#9368 = EDGE_CURVE ( 'NONE', #17098, #8171, #10587, .T. ) ;
#9369 = VECTOR ( 'NONE', #4035, 1000.000000000000000 ) ;
#9370 = EDGE_LOOP ( 'NONE', ( #2823, #15080, #11237, #1358 ) ) ;
#9371 = CARTESIAN_POINT ( 'NONE',  ( -9.999999999999994671, 20.00000000000001421, 9.999999999999998224 ) ) ;
#9372 = ADVANCED_FACE ( 'NONE', ( #4817 ), #3255, .T. ) ;
#9373 = EDGE_CURVE ( 'NONE', #2700, #5469, #11118, .T. ) ;
#9374 = CARTESIAN_POINT ( 'NONE',  ( 50.02271294988512551, 50.49948385550240459, 7.000000000000000888 ) ) ;
#9375 = DIRECTION ( 'NONE',  ( -0.000000000000000000, -0.000000000000000000, 1.000000000000000000 ) ) ;
#9376 = EDGE_LOOP ( 'NONE', ( #16985, #11950, #9828, #7067 ) ) ;
#9377 = LINE ( 'NONE', #8007, #7069 ) ;
#9378 = AXIS2_PLACEMENT_3D ( 'NONE', #10297, #11474, #17484 ) ;
#9379 = EDGE_CURVE ( 'NONE', #12892, #6434, #15298, .T. ) ;
#9380 = ADVANCED_FACE ( 'NONE', ( #4435, #2966 ), #8930, .T. ) ;
#9381 = VERTEX_POINT ( 'NONE', #492 ) ;
#9382 = CARTESIAN_POINT ( 'NONE',  ( 45.90387839640208512, 64.30051614449766362, -5.676469297603124353 ) ) ;
#9383 = EDGE_LOOP ( 'NONE', ( #13602, #10458, #3782, #8067 ) ) ;
#9384 = EDGE_CURVE ( 'NONE', #9187, #6420, #7078, .T. ) ;
#9385 = DIRECTION ( 'NONE',  ( 0.000000000000000000, -0.000000000000000000, 1.000000000000000000 ) ) ;
#9386 = CARTESIAN_POINT ( 'NONE',  ( 20.00000000000000000, -20.00000000000000000, -20.00000000000000000 ) ) ;
#9387 = AXIS2_PLACEMENT_3D ( 'NONE', #5839, #1527, #13285 ) ;
#9388 = CARTESIAN_POINT ( 'NONE',  ( 56.30877334542961421, 55.00051614449766646, 0.02388180880515774693 ) ) ;
#9389 = CARTESIAN_POINT ( 'NONE',  ( 0.08165819712376902462, 3.720292241887087403, -3.556264818047239817 ) ) ;
#9390 = DIRECTION ( 'NONE',  ( -0.000000000000000000, -0.000000000000000000, 1.000000000000000000 ) ) ;
#9391 = CARTESIAN_POINT ( 'NONE',  ( 12.54977455159135502, -35.57251292194776227, 0.000000000000000000 ) ) ;
#9392 = VECTOR ( 'NONE', #10249, 1000.000000000000000 ) ;
#9393 = EDGE_CURVE ( 'NONE', #17702, #3410, #10874, .T. ) ;
#9394 = CARTESIAN_POINT ( 'NONE',  ( 56.79116909180259398, 57.20051614449766220, 4.963592699178938972 ) ) ;
#9395 = ADVANCED_FACE ( 'NONE', ( #18360 ), #11156, .F. ) ;
#9396 = AXIS2_PLACEMENT_3D ( 'NONE', #6550, #10772, #14090 ) ;
#9397 = CIRCLE ( 'NONE', #12526, 2.396904916527700102 ) ;
#9398 = VERTEX_POINT ( 'NONE', #690 ) ;
#9399 = ORIENTED_EDGE ( 'NONE', *, *, #3648, .F. ) ;
#9400 = CARTESIAN_POINT ( 'NONE',  ( 0.3108895250735811966, -2.416698868092462149, 4.999999999999999112 ) ) ;
#9401 = SURFACE_STYLE_USAGE ( .BOTH. , #3439 ) ;
#9402 = ORIENTED_EDGE ( 'NONE', *, *, #16129, .T. ) ;
#9403 = FILL_AREA_STYLE_COLOUR ( '', #17819 ) ;
#9404 = CONTEXT_DEPENDENT_SHAPE_REPRESENTATION ( #11276, #11319 ) ;
#9405 = AXIS2_PLACEMENT_3D ( 'NONE', #11983, #8652, #2891 ) ;
#9406 = ORIENTED_EDGE ( 'NONE', *, *, #12392, .F. ) ;
#9407 = CYLINDRICAL_SURFACE ( 'NONE', #13925, 20.00000000000000000 ) ;
#9408 = DIRECTION ( 'NONE',  ( -0.000000000000000000, 0.000000000000000000, -1.000000000000000000 ) ) ;
#9409 =( BOUNDED_SURFACE ( )  B_SPLINE_SURFACE ( 3, 2, ( 
 ( #18754, #6772, #8335 ),
 ( #5496, #15800, #5300 ),
 ( #12658, #18859, #6865 ),
 ( #2588, #8439, #17283 ),
 ( #11466, #3844, #11174 ),
 ( #5203, #9706, #9804 ) ),
 .UNSPECIFIED., .F., .F., .F. ) 
 B_SPLINE_SURFACE_WITH_KNOTS ( ( 4, 2, 4 ),
 ( 3, 3 ),
 ( 0.02367865728600889938, 0.02663179453327095547, 0.02958493178053301503 ),
 ( 0.000000000000000000, 1.000000000000000000 ),
 .UNSPECIFIED. ) 
 GEOMETRIC_REPRESENTATION_ITEM ( )  RATIONAL_B_SPLINE_SURFACE ( (
 ( 1.000000000000000000, 0.8047781103519390244, 1.000000000000000000),
 ( 1.000000000000000000, 0.8123785825980075481, 1.000000000000000000),
 ( 1.000000000000000000, 0.8190671539288042480, 1.000000000000000000),
 ( 1.000000000000000000, 0.8192352255335092481, 1.000000000000000000),
 ( 1.000000000000000000, 0.8126129676835915916, 1.000000000000000000),
 ( 1.000000000000000000, 0.8047712537969718971, 1.000000000000000000) ) ) 
 REPRESENTATION_ITEM ( '' )  SURFACE ( )  );
#9410 = AXIS2_PLACEMENT_3D ( 'NONE', #3929, #4025, #7052 ) ;
#9411 = CARTESIAN_POINT ( 'NONE',  ( 4.158233816354936607, -0.4370479853238358192, -9.000000000000000000 ) ) ;
#9412 = CIRCLE ( 'NONE', #8488, 2.055000000000000160 ) ;
#9413 = CYLINDRICAL_SURFACE ( 'NONE', #16131, 2.000000000000001776 ) ;
#9414 = CIRCLE ( 'NONE', #14426, 5.400000000000000355 ) ;
#9415 = CIRCLE ( 'NONE', #15071, 5.000000000000000888 ) ;
#9416 = DIRECTION ( 'NONE',  ( -9.710251638871371392E-17, -5.969973981896233748E-17, -1.000000000000000000 ) ) ;
#9417 = DIRECTION ( 'NONE',  ( -1.000000000000000000, 0.000000000000000000, 0.000000000000000000 ) ) ;
#9418 = CARTESIAN_POINT ( 'NONE',  ( 53.54508667620428497, 46.29948385550240886, 4.840751629271157874 ) ) ;
#9419 = ADVANCED_BREP_SHAPE_REPRESENTATION ( '', ( #1938, #10359 ), #1294 ) ;
#9420 = FACE_OUTER_BOUND ( 'NONE', #12137, .T. ) ;
#9421 = CARTESIAN_POINT ( 'NONE',  ( 42.38452918213188525, 59.09948385550240602, -2.450534656007040013 ) ) ;
#9422 = CARTESIAN_POINT ( 'NONE',  ( 45.86712807150329496, 59.70051614449766220, 5.649768623646139964 ) ) ;
#9423 = CARTESIAN_POINT ( 'NONE',  ( 1.267864665261691752E-11, -20.00000000000000000, 9.999999999999998224 ) ) ;
#9424 = DIRECTION ( 'NONE',  ( 1.000000000000000000, -0.000000000000000000, -0.000000000000000000 ) ) ;
#9425 = AXIS2_PLACEMENT_3D ( 'NONE', #11437, #1252, #16159 ) ;
#9426 = ORIENTED_EDGE ( 'NONE', *, *, #5015, .T. ) ;
#9427 = AXIS2_PLACEMENT_3D ( 'NONE', #4032, #4129, #6768 ) ;
#9428 = AXIS2_PLACEMENT_3D ( 'NONE', #13786, #12222, #4783 ) ;
#9429 = DIRECTION ( 'NONE',  ( 0.000000000000000000, 0.000000000000000000, 1.000000000000000000 ) ) ;
#9430 = CARTESIAN_POINT ( 'NONE',  ( 47.70284917648459810, 47.60051614449766078, 6.992620115222797139 ) ) ;
#9431 = CARTESIAN_POINT ( 'NONE',  ( 47.70284917648453415, 63.39948385550240317, -6.992620115222774047 ) ) ;
#9432 = CYLINDRICAL_SURFACE ( 'NONE', #17455, 1.000000000000000888 ) ;
#9433 = ORIENTED_EDGE ( 'NONE', *, *, #18391, .F. ) ;
#9434 = CARTESIAN_POINT ( 'NONE',  ( 1.000000000000002442, -20.00000000000000000, -9.000000000000001776 ) ) ;
#9435 = CARTESIAN_POINT ( 'NONE',  ( 2.449293598294706513E-15, -20.00000000000000000, -50.00000000000000000 ) ) ;
#9436 = ADVANCED_FACE ( 'NONE', ( #6560 ), #15586, .T. ) ;
#9437 = CARTESIAN_POINT ( 'NONE',  ( 55.11794222512601493, 62.19948385550240744, 3.688883143319541702 ) ) ;
#9438 = CARTESIAN_POINT ( 'NONE',  ( 6.534838248920896930, -2.951765777552406878, 5.112608298763836601 ) ) ;
#9439 = CARTESIAN_POINT ( 'NONE',  ( 56.65037692655918988, 45.89948385550240317, -2.184720259617163762 ) ) ;
#9440 = LINE ( 'NONE', #6493, #16104 ) ;
#9441 = CARTESIAN_POINT ( 'NONE',  ( 43.20883090819742023, 60.20051614449766220, -4.963592699178938972 ) ) ;
#9442 = EDGE_CURVE ( 'NONE', #13074, #2657, #3001, .T. ) ;
#9443 = CARTESIAN_POINT ( 'NONE',  ( 50.02271294988506156, 64.50051614449766646, -6.000000000000000888 ) ) ;
#9444 = CIRCLE ( 'NONE', #16679, 5.384454397937118664 ) ;
#9445 = DIRECTION ( 'NONE',  ( 0.000000000000000000, -1.000000000000000000, 1.345283343056720273E-15 ) ) ;
#9446 = CARTESIAN_POINT ( 'NONE',  ( 6.390820841722131718, -2.823237767533154141, -5.110008744785255352 ) ) ;
#9447 = VERTEX_POINT ( 'NONE', #17164 ) ;
#9448 = EDGE_LOOP ( 'NONE', ( #96, #7701, #756, #14497 ) ) ;
#9449 = DIRECTION ( 'NONE',  ( 1.000000000000000000, -1.734723475976807341E-16, -0.000000000000000000 ) ) ;
#9450 = ORIENTED_EDGE ( 'NONE', *, *, #14348, .T. ) ;
#9451 = B_SPLINE_CURVE_WITH_KNOTS ( 'NONE', 3,
 ( #12114, #13682, #17958, #1832, #7800, #18315 ),
 .UNSPECIFIED., .F., .F.,
 ( 4, 2, 4 ),
 ( 0.002365888236227995517, 0.003551327329835084114, 0.004736766423442172712 ),
 .UNSPECIFIED. ) ;
#9452 = DIRECTION ( 'NONE',  ( -0.000000000000000000, -0.000000000000000000, -1.000000000000000000 ) ) ;
#9453 = B_SPLINE_CURVE_WITH_KNOTS ( 'NONE', 3,
 ( #2867, #5791, #2770, #10188, #8728, #11666, #16094, #2677 ),
 .UNSPECIFIED., .F., .F.,
 ( 4, 2, 2, 4 ),
 ( 0.002921158011986727237, 0.003648658599403079624, 0.004376159186819432445, 0.005831160361652135485 ),
 .UNSPECIFIED. ) ;
#9454 = ORIENTED_EDGE ( 'NONE', *, *, #1734, .F. ) ;
#9455 = DIRECTION ( 'NONE',  ( 0.000000000000000000, 0.000000000000000000, 1.000000000000000000 ) ) ;
#9456 = CARTESIAN_POINT ( 'NONE',  ( 44.05948171654949874, 54.79948385550240886, 4.345558710429104465 ) ) ;
#9457 = VERTEX_POINT ( 'NONE', #5284 ) ;
#9458 = CARTESIAN_POINT ( 'NONE',  ( 0.000000000000000000, 0.000000000000000000, -4.974599999999998801 ) ) ;
#9459 = ORIENTED_EDGE ( 'NONE', *, *, #7729, .F. ) ;
#9460 = CARTESIAN_POINT ( 'NONE',  ( 50.02271294988513972, 50.49948385550239749, 8.000000000000001776 ) ) ;
#9461 = CARTESIAN_POINT ( 'NONE',  ( 62.49999999999998579, 45.00000000000001421, 5.000000000000000000 ) ) ;
#9462 = CARTESIAN_POINT ( 'NONE',  ( 55.69932041026404335, 45.89948385550240317, -1.875703265242203432 ) ) ;
#9463 = CARTESIAN_POINT ( 'NONE',  ( 4.158921614371307918, 4.076055977742304215, -0.05993604794450364120 ) ) ;
#9464 = FACE_OUTER_BOUND ( 'NONE', #10274, .T. ) ;
#9465 = CARTESIAN_POINT ( 'NONE',  ( 52.29715082351538769, 62.60051614449766078, -6.992620115222796251 ) ) ;
#9466 = DIRECTION ( 'NONE',  ( -0.000000000000000000, -0.000000000000000000, -1.000000000000000000 ) ) ;
#9467 = CARTESIAN_POINT ( 'NONE',  ( 56.66441430157296821, 56.09948385550240602, 2.141517661632100111 ) ) ;
#9468 = DIRECTION ( 'NONE',  ( 2.191393683118470056E-17, 7.538405132783724027E-17, 1.000000000000000000 ) ) ;
#9469 = ORIENTED_EDGE ( 'NONE', *, *, #13338, .F. ) ;
#9470 = AXIS2_PLACEMENT_3D ( 'NONE', #16490, #10683, #11645 ) ;
#9471 = EDGE_LOOP ( 'NONE', ( #7479, #15874, #6734, #1443 ) ) ;
#9472 = CARTESIAN_POINT ( 'NONE',  ( -154.9999999999999716, -6.999999999999993783, 15.00000000000000000 ) ) ;
#9473 = CARTESIAN_POINT ( 'NONE',  ( 44.03140696652192787, 53.19948385550238612, -4.306917132069425058 ) ) ;
#9474 = CARTESIAN_POINT ( 'NONE',  ( 20.00000000000000000, -20.00000000000000000, -20.00000000000000000 ) ) ;
#9475 = ORIENTED_EDGE ( 'NONE', *, *, #4076, .T. ) ;
#9476 = CARTESIAN_POINT ( 'NONE',  ( 0.02993401039713891598, -3.373851915354620257, -1.156317065392238774 ) ) ;
#9477 = EDGE_LOOP ( 'NONE', ( #1145, #5206, #9002, #16637, #11288 ) ) ;
#9478 = LINE ( 'NONE', #5166, #10046 ) ;
#9479 = ORIENTED_EDGE ( 'NONE', *, *, #18031, .T. ) ;
#9480 = EDGE_CURVE ( 'NONE', #2843, #17538, #9551, .T. ) ;
#9481 = CARTESIAN_POINT ( 'NONE',  ( 43.33558569842703179, 47.09948385550240602, -2.141517661632099223 ) ) ;
#9482 = UNCERTAINTY_MEASURE_WITH_UNIT (LENGTH_MEASURE( 1.000000000000000082E-05 ), #399, 'distance_accuracy_value', 'NONE');
#9483 = DIRECTION ( 'NONE',  ( 0.000000000000000000, 0.000000000000000000, 1.000000000000000000 ) ) ;
#9484 = CARTESIAN_POINT ( 'NONE',  ( 55.69932041026405045, 63.10051614449766078, 1.875703265242156359 ) ) ;
#9485 = DIRECTION ( 'NONE',  ( -0.1045284632676563297, 0.9945218953682731788, 0.000000000000000000 ) ) ;
#9486 = DIRECTION ( 'NONE',  ( 1.000000000000000000, 0.000000000000000000, 0.000000000000000000 ) ) ;
#9487 = DIRECTION ( 'NONE',  ( -0.5000000000000061062, 0.000000000000000000, 0.8660254037844351549 ) ) ;
#9488 = CARTESIAN_POINT ( 'NONE',  ( 56.79116909180259398, 61.20051614449766220, 4.963592699178938972 ) ) ;
#9489 = ORIENTED_EDGE ( 'NONE', *, *, #3283, .T. ) ;
#9490 = VERTEX_POINT ( 'NONE', #18646 ) ;
#9491 = CARTESIAN_POINT ( 'NONE',  ( 2.449293598294706513E-15, -20.00000000000000000, 9.000000000000000000 ) ) ;
#9492 = DIRECTION ( 'NONE',  ( -0.000000000000000000, -0.000000000000000000, -1.000000000000000000 ) ) ;
#9493 = ADVANCED_FACE ( 'NONE', ( #3536 ), #9407, .T. ) ;
#9494 = ORIENTED_EDGE ( 'NONE', *, *, #404, .T. ) ;
#9495 = CARTESIAN_POINT ( 'NONE',  ( -9.999999999999996447, 25.00000000000001776, 15.00000000000000000 ) ) ;
#9496 = CARTESIAN_POINT ( 'NONE',  ( 0.2499999999999966416, -8.096141056083448362, 0.000000000000000000 ) ) ;
#9497 = ORIENTED_EDGE ( 'NONE', *, *, #2409, .F. ) ;
#9498 = EDGE_CURVE ( 'NONE', #10423, #6664, #15731, .T. ) ;
#9499 = FACE_OUTER_BOUND ( 'NONE', #3599, .T. ) ;
#9500 = UNCERTAINTY_MEASURE_WITH_UNIT (LENGTH_MEASURE( 1.000000000000000082E-05 ), #7803, 'distance_accuracy_value', 'NONE');
#9501 = EDGE_CURVE ( 'NONE', #337, #9866, #1114, .T. ) ;
#9502 = CARTESIAN_POINT ( 'NONE',  ( -1.149999999999998135, 5.021051876504148371E-16, 4.100000000000000533 ) ) ;
#9503 = CIRCLE ( 'NONE', #3572, 0.5999999999999998668 ) ;
#9504 = DIRECTION ( 'NONE',  ( 0.000000000000000000, 8.673617379884036458E-16, 1.000000000000000000 ) ) ;
#9505 = LINE ( 'NONE', #16788, #19375 ) ;
#9506 = CARTESIAN_POINT ( 'NONE',  ( 45.90387839640214196, 64.69948385550240744, 5.676469297603166098 ) ) ;
#9507 = CARTESIAN_POINT ( 'NONE',  ( -9.037824375505429941, -37.84146099840256738, 9.000000000000000000 ) ) ;
#9508 = CARTESIAN_POINT ( 'NONE',  ( 58.41169779390614281, 57.99948385550241170, -0.02388180880523160798 ) ) ;
#9509 = CARTESIAN_POINT ( 'NONE',  ( 47.74827507625469281, 60.40051614449767214, -7.007379884777203749 ) ) ;
#9510 = EDGE_CURVE ( 'NONE', #11082, #4891, #8624, .T. ) ;
#9511 = EDGE_CURVE ( 'NONE', #3923, #2538, #10182, .T. ) ;
#9512 = DIRECTION ( 'NONE',  ( -9.858538378746663627E-23, 5.031452844637890958E-23, -1.000000000000000000 ) ) ;
#9513 = LINE ( 'NONE', #6203, #4721 ) ;
#9514 = B_SPLINE_CURVE_WITH_KNOTS ( 'NONE', 3,
 ( #11561, #3839, #19151, #15894, #9894 ),
 .UNSPECIFIED., .F., .F.,
 ( 4, 1, 4 ),
 ( 0.000000000000000000, 0.002020725942163690506, 0.004041451884327381013 ),
 .UNSPECIFIED. ) ;
#9515 = AXIS2_PLACEMENT_3D ( 'NONE', #6398, #6592, #9720 ) ;
#9516 = EDGE_CURVE ( 'NONE', #17116, #2487, #12696, .T. ) ;
#9517 = FILL_AREA_STYLE_COLOUR ( '', #1231 ) ;
#9518 = ORIENTED_EDGE ( 'NONE', *, *, #10216, .T. ) ;
#9519 = VECTOR ( 'NONE', #1184, 1000.000000000000000 ) ;
#9520 = DIRECTION ( 'NONE',  ( 0.000000000000000000, 0.4999999999999989453, -0.8660254037844391517 ) ) ;
#9521 = DIRECTION ( 'NONE',  ( -1.000000000000000000, 9.251858538542972814E-17, -0.000000000000000000 ) ) ;
#9522 = CARTESIAN_POINT ( 'NONE',  ( 42.63976443033212149, 46.00051614449765225, -0.02388180880514948964 ) ) ;
#9523 = CARTESIAN_POINT ( 'NONE',  ( 4.132952817037866211, -2.031684012687259511, 3.518979934899751250 ) ) ;
#9524 = CARTESIAN_POINT ( 'NONE',  ( 4.000000000000000000, 2.309401076758497151, -5.000000000000000000 ) ) ;
#9525 = VERTEX_POINT ( 'NONE', #18450 ) ;
#9526 = DIRECTION ( 'NONE',  ( -0.7779254092217071648, -0.6283566325640553840, 0.000000000000000000 ) ) ;
#9527 = FACE_OUTER_BOUND ( 'NONE', #11652, .T. ) ;
#9528 = CARTESIAN_POINT ( 'NONE',  ( 53.50833635130540955, 63.69948385550240033, -4.867452303228209765 ) ) ;
#9529 = CARTESIAN_POINT ( 'NONE',  ( 4.101954839143059139, -2.368264730582948285, -3.681130640444269631 ) ) ;
#9530 = DIRECTION ( 'NONE',  ( -0.000000000000000000, 0.000000000000000000, -1.000000000000000000 ) ) ;
#9531 = CARTESIAN_POINT ( 'NONE',  ( 58.41169779390614281, 63.00051614449766646, 0.02388180880515032231 ) ) ;
#9532 = VECTOR ( 'NONE', #12725, 1000.000000000000000 ) ;
#9533 = CARTESIAN_POINT ( 'NONE',  ( 46.49166364869456913, 64.30051614449766362, -4.867452303228181343 ) ) ;
#9534 = CARTESIAN_POINT ( 'NONE',  ( -74.99999999999997158, -1.000000000000000000, 6.000000000000001776 ) ) ;
#9535 = CARTESIAN_POINT ( 'NONE',  ( 6.357976367241527704, -5.421935536068480666, -0.8264656814046078548 ) ) ;
#9536 = EDGE_LOOP ( 'NONE', ( #8521, #10640, #8512, #6277, #3517 ) ) ;
#9537 = ORIENTED_EDGE ( 'NONE', *, *, #11095, .T. ) ;
#9538 = DIRECTION ( 'NONE',  ( 0.000000000000000000, 0.000000000000000000, 1.000000000000000000 ) ) ;
#9539 = VERTEX_POINT ( 'NONE', #18735 ) ;
#9540 = EDGE_CURVE ( 'NONE', #14765, #1266, #3626, .T. ) ;
#9541 = FACE_OUTER_BOUND ( 'NONE', #14419, .T. ) ;
#9542 = EDGE_LOOP ( 'NONE', ( #4706, #9548, #17796, #90 ) ) ;
#9543 = CARTESIAN_POINT ( 'NONE',  ( 4.071447262713888016, -2.020725942163694722, -3.499999999999999556 ) ) ;
#9544 = EDGE_CURVE ( 'NONE', #1321, #10552, #2056, .T. ) ;
#9545 = CARTESIAN_POINT ( 'NONE',  ( 43.33558569842703179, 55.09948385550241312, -2.141517661632099223 ) ) ;
#9546 = VERTEX_POINT ( 'NONE', #6463 ) ;
#9547 = DIRECTION ( 'NONE',  ( -1.000000000000000000, 0.000000000000000000, 0.000000000000000000 ) ) ;
#9548 = ORIENTED_EDGE ( 'NONE', *, *, #18047, .F. ) ;
#9549 = CARTESIAN_POINT ( 'NONE',  ( 57.60143344285433642, 49.89948385550241028, -2.493737253992118319 ) ) ;
#9550 = CARTESIAN_POINT ( 'NONE',  ( 3.948111298835276894, -0.6968132764964354298, -3.500000000000154987 ) ) ;
#9551 = CIRCLE ( 'NONE', #12367, 5.899999999999999467 ) ;
#9552 = CARTESIAN_POINT ( 'NONE',  ( 52.29715082351547295, 62.39948385550239607, 6.992620115222774047 ) ) ;
#9553 = FACE_OUTER_BOUND ( 'NONE', #17740, .T. ) ;
#9554 = CARTESIAN_POINT ( 'NONE',  ( 4.170895651974851681, -4.109780709045220526, -1.251026243406537913E-13 ) ) ;
#9555 = CARTESIAN_POINT ( 'NONE',  ( 45.90387839640208512, 60.30051614449766362, -5.676469297603124353 ) ) ;
#9556=STYLED_ITEM('',(#19454),#2264);
#9557 = CARTESIAN_POINT ( 'NONE',  ( 54.13287192849676188, 56.29948385550240175, 5.649768623646098220 ) ) ;
#9558 = LINE ( 'NONE', #3225, #5351 ) ;
#9559 = CARTESIAN_POINT ( 'NONE',  ( -4.000000000000000000, -1.942223658245633811, -0.3516579909967644246 ) ) ;
#9560 = ORIENTED_EDGE ( 'NONE', *, *, #10126, .F. ) ;
#9561 = ORIENTED_EDGE ( 'NONE', *, *, #9308, .F. ) ;
#9562 = DIRECTION ( 'NONE',  ( 0.000000000000000000, 0.000000000000000000, 1.000000000000000000 ) ) ;
#9563 =( LENGTH_UNIT ( ) NAMED_UNIT ( * ) SI_UNIT ( .MILLI., .METRE. ) );
#9564 = AXIS2_PLACEMENT_3D ( 'NONE', #12419, #5164, #14079 ) ;
#9565 = EDGE_CURVE ( 'NONE', #7050, #11034, #4996, .T. ) ;
#9566 = CARTESIAN_POINT ( 'NONE',  ( 55.96859303347804371, 50.19948385550240744, 4.306917132069425946 ) ) ;
#9567 = CARTESIAN_POINT ( 'NONE',  ( -0.1481481481481481122, -4.797713218419819903, 0.000000000000000000 ) ) ;
#9568 = ORIENTED_EDGE ( 'NONE', *, *, #13480, .F. ) ;
#9569 = ORIENTED_EDGE ( 'NONE', *, *, #18283, .T. ) ;
#9570 = CARTESIAN_POINT ( 'NONE',  ( -155.0712099064782876, -18.99936609342274352, 17.00000000000000000 ) ) ;
#9571 = AXIS2_PLACEMENT_3D ( 'NONE', #993, #6961, #12940 ) ;
#9572 = ORIENTED_EDGE ( 'NONE', *, *, #883, .F. ) ;
#9573 = DIRECTION ( 'NONE',  ( -0.04542589977017699732, 0.9989677110047501252, 0.000000000000000000 ) ) ;
#9574 = ORIENTED_EDGE ( 'NONE', *, *, #4137, .F. ) ;
#9575 = DIRECTION ( 'NONE',  ( -0.000000000000000000, -0.000000000000000000, 1.000000000000000000 ) ) ;
#9576 = CARTESIAN_POINT ( 'NONE',  ( 0.3126073911696427010, 4.041451884327382338, -6.521455134176256610E-17 ) ) ;
#9577 = CARTESIAN_POINT ( 'NONE',  ( 49.97728705011494554, 59.50051614449765935, 6.000000000000000888 ) ) ;
#9578 = DIRECTION ( 'NONE',  ( -9.710251638871371392E-17, -5.969973981896234981E-17, -1.000000000000000000 ) ) ;
#9579 = DIRECTION ( 'NONE',  ( 1.000000000000000000, 0.000000000000000000, 0.000000000000000000 ) ) ;
#9580 = CARTESIAN_POINT ( 'NONE',  ( 6.355827204229362870, 5.411702751981843917, -0.8440485055075606091 ) ) ;
#9581 = CARTESIAN_POINT ( 'NONE',  ( 47.37792948025170858, 61.60051614449765367, 7.992620115222797139 ) ) ;
#9582 = ORIENTED_EDGE ( 'NONE', *, *, #9069, .T. ) ;
#9583 = ORIENTED_EDGE ( 'NONE', *, *, #9324, .F. ) ;
#9584 = LINE ( 'NONE', #15390, #18740 ) ;
#9585 = CYLINDRICAL_SURFACE ( 'NONE', #4065, 3.500000000000000000 ) ;
#9586 = ORIENTED_EDGE ( 'NONE', *, *, #8508, .T. ) ;
#9587 = VECTOR ( 'NONE', #11091, 1000.000000000000000 ) ;
#9588 = CARTESIAN_POINT ( 'NONE',  ( 6.244297270354684848, -1.798312406574552930E-11, -5.105276777067894400 ) ) ;
#9589 = PLANE ( 'NONE',  #13778 ) ;
#9590 = ORIENTED_EDGE ( 'NONE', *, *, #19102, .T. ) ;
#9591 = CLOSED_SHELL ( 'NONE', ( #5552, #10916, #12922, #5182, #1797, #1603, #14307, #3941, #17430, #12269, #5192, #18412, #8192, #3002, #7495, #7108, #3227, #9138, #15316, #18541, #8802, #8851, #11420, #12028, #17323, #13033, #13339, #9493, #14063, #16240, #12371, #10507, #7267, #9754, #4375, #6984, #4293, #16543, #9879, #13459, #5620, #8300, #17971, #10364, #10042, #13347, #4724, #14597, #3310, #19197, #11230, #8925, #17479, #6497, #10816, #16898, #11471, #15260, #7894, #10085, #15258, #7245, #3892, #7830, #18641, #5702, #1354, #4171, #3068, #13464, #10367, #3816, #4860, #930, #12121, #12136, #10727, #2827, #18808, #12488, #18299, #14530, #7138 ) ) ;
#9592 = CARTESIAN_POINT ( 'NONE',  ( 2.000000000000000000, 1.773042676681340524, -2.059984127722458425E-15 ) ) ;
#9593 = FACE_OUTER_BOUND ( 'NONE', #6044, .T. ) ;
#9594 = CARTESIAN_POINT ( 'NONE',  ( -30.00000000000000000, -40.00000000000000000, -5.999999999999998224 ) ) ;
#9595 = AXIS2_PLACEMENT_3D ( 'NONE', #5929, #11890, #9152 ) ;
#9596 = FACE_BOUND ( 'NONE', #17040, .T. ) ;
#9597 = CARTESIAN_POINT ( 'NONE',  ( 45.90387839640214196, 62.69948385550240744, 5.676469297603166098 ) ) ;
#9598 = DIRECTION ( 'NONE',  ( -1.000000000000000000, 0.000000000000000000, 0.000000000000000000 ) ) ;
#9599 = AXIS2_PLACEMENT_3D ( 'NONE', #5463, #11050, #18828 ) ;
#9600 = CARTESIAN_POINT ( 'NONE',  ( 52.62207051974839089, 58.39948385550241028, 7.992620115222770494 ) ) ;
#9601 = CARTESIAN_POINT ( 'NONE',  ( 52.29715082351538769, 58.60051614449766078, -6.992620115222796251 ) ) ;
#9602 = CARTESIAN_POINT ( 'NONE',  ( 49.97728705011488159, 65.49948385550240459, -7.000000000000000888 ) ) ;
#9603 = DIRECTION ( 'NONE',  ( 1.000000000000000000, 0.000000000000000000, 0.000000000000000000 ) ) ;
#9604 = ADVANCED_FACE ( 'NONE', ( #2664 ), #12067, .T. ) ;
#9605 = DIRECTION ( 'NONE',  ( 1.000000000000000000, 0.000000000000000000, 0.000000000000000000 ) ) ;
#9606 = CIRCLE ( 'NONE', #11137, 8.099999999999999645 ) ;
#9607 = ORIENTED_EDGE ( 'NONE', *, *, #17054, .T. ) ;
#9608 = DIRECTION ( 'NONE',  ( 1.000000000000000000, 0.000000000000000000, 0.000000000000000000 ) ) ;
#9609 = EDGE_CURVE ( 'NONE', #7321, #6641, #13009, .T. ) ;
#9610 = AXIS2_PLACEMENT_3D ( 'NONE', #17653, #8709, #1075 ) ;
#9611 = CARTESIAN_POINT ( 'NONE',  ( -3.309651814758565180, -5.455921364805393026, -1.000000000000000000 ) ) ;
#9612 = AXIS2_PLACEMENT_3D ( 'NONE', #10328, #14548, #12988 ) ;
#9613 = CARTESIAN_POINT ( 'NONE',  ( -74.99999999999997158, -6.999999999999989342, 10.00000000000000000 ) ) ;
#9614 = EDGE_CURVE ( 'NONE', #10315, #5073, #2569, .T. ) ;
#9615 = EDGE_CURVE ( 'NONE', #5826, #9274, #11444, .T. ) ;
#9616 = CARTESIAN_POINT ( 'NONE',  ( -74.99999999999997158, 20.00000000000001421, -15.00000000000000000 ) ) ;
#9617 = LINE ( 'NONE', #10714, #11476 ) ;
#9618 = ORIENTED_EDGE ( 'NONE', *, *, #10945, .T. ) ;
#9619 = CARTESIAN_POINT ( 'NONE',  ( 5.000000000000003553, -20.00000000000000000, 15.00000000000000355 ) ) ;
#9620 = DIRECTION ( 'NONE',  ( 1.000000000000000000, 0.000000000000000000, 0.000000000000000000 ) ) ;
#9621 = EDGE_CURVE ( 'NONE', #10976, #13559, #7383, .T. ) ;
#9622 = CARTESIAN_POINT ( 'NONE',  ( -74.99999999999997158, 2.999999999999999112, -5.999999999999998224 ) ) ;
#9623 = CARTESIAN_POINT ( 'NONE',  ( 50.02271294988512551, 46.49948385550240459, 7.000000000000000888 ) ) ;
#9624 = CARTESIAN_POINT ( 'NONE',  ( -2.000000000000007550, -3.464101615137749945, 0.000000000000000000 ) ) ;
#9625 = CIRCLE ( 'NONE', #1823, 2.649999999999985700 ) ;
#9626 = CARTESIAN_POINT ( 'NONE',  ( 47.37792948025170858, 59.60051614449765367, 7.992620115222797139 ) ) ;
#9627 = CARTESIAN_POINT ( 'NONE',  ( 55.08986747509849380, 61.20051614449766220, 3.727524721679155384 ) ) ;
#9628 = LINE ( 'NONE', #14443, #12861 ) ;
#9629 = CARTESIAN_POINT ( 'NONE',  ( 6.245835795331710294, -1.036512332922514767, 5.105321605219339531 ) ) ;
#9631 = VERTEX_POINT ( 'NONE', #14689 ) ;
#9630 = EDGE_CURVE ( 'NONE', #9875, #5600, #5815, .T. ) ;
#9632 = EDGE_CURVE ( 'NONE', #1857, #17716, #8637, .T. ) ;
#9633 = ORIENTED_EDGE ( 'NONE', *, *, #18347, .T. ) ;
#9634 = EDGE_LOOP ( 'NONE', ( #6365, #12125, #14607, #8971 ) ) ;
#9635 = DIRECTION ( 'NONE',  ( 4.082155997157843695E-16, -1.000000000000000000, 0.000000000000000000 ) ) ;
#9636 = ORIENTED_EDGE ( 'NONE', *, *, #9762, .T. ) ;
#9637 = DIRECTION ( 'NONE',  ( -0.000000000000000000, -0.000000000000000000, 1.000000000000000000 ) ) ;
#9638 = VERTEX_POINT ( 'NONE', #1277 ) ;
#9639 = DIRECTION ( 'NONE',  ( -1.000000000000000000, 0.000000000000000000, 0.000000000000000000 ) ) ;
#9640 = AXIS2_PLACEMENT_3D ( 'NONE', #5874, #93, #13607 ) ;
#9641 = CARTESIAN_POINT ( 'NONE',  ( 57.36023556966787851, 55.99948385550239749, -0.02388180880522424582 ) ) ;
#9642 = VECTOR ( 'NONE', #6948, 1000.000000000000114 ) ;
#9643 = ORIENTED_EDGE ( 'NONE', *, *, #4413, .T. ) ;
#9644 = CARTESIAN_POINT ( 'NONE',  ( 6.420058897733093239, -2.891482565094600776, -5.008194711943422917 ) ) ;
#9645 = VERTEX_POINT ( 'NONE', #10084 ) ;
#9646 = APPLICATION_CONTEXT ( 'automotive_design' ) ;
#9647 = CARTESIAN_POINT ( 'NONE',  ( 45.27934281921075410, 53.29948385550240886, -6.458785618021043895 ) ) ;
#9648 = CYLINDRICAL_SURFACE ( 'NONE', #3882, 2.396904916527699214 ) ;
#9649 = CARTESIAN_POINT ( 'NONE',  ( 44.03140696652192787, 63.19948385550240744, -4.306917132069425058 ) ) ;
#9650 = CARTESIAN_POINT ( 'NONE',  ( -18.02113032590308705, -13.81966011250110249, -9.000000000000000000 ) ) ;
#9651 = DIRECTION ( 'NONE',  ( -0.9992259981072103558, -0.03933706530295846826, 2.486236275248362725E-17 ) ) ;
#9652 = CARTESIAN_POINT ( 'NONE',  ( 43.33558569842706021, 59.90051614449766504, 2.141517661632167169 ) ) ;
#9653 = CARTESIAN_POINT ( 'NONE',  ( 55.08986747509847248, 63.79948385550241596, -3.727524721679197572 ) ) ;
#9654 = CARTESIAN_POINT ( 'NONE',  ( 50.02271294988512551, 56.49948385550240459, 7.000000000000000888 ) ) ;
#9655 = CARTESIAN_POINT ( 'NONE',  ( 4.211140560182196957, 2.431303136016536470, -3.745885042887433514 ) ) ;
#9656 = LINE ( 'NONE', #15105, #8128 ) ;
#9657 = VECTOR ( 'NONE', #14786, 1000.000000000000000 ) ;
#9658 = ORIENTED_EDGE ( 'NONE', *, *, #9162, .T. ) ;
#9659 = CIRCLE ( 'NONE', #14677, 10.00000000000000888 ) ;
#9660 = EDGE_LOOP ( 'NONE', ( #15880, #5314, #7596, #18503 ) ) ;
#9661 = DIRECTION ( 'NONE',  ( 0.000000000000000000, 1.000000000000000000, -1.224646799147353207E-16 ) ) ;
#9662 = CARTESIAN_POINT ( 'NONE',  ( 50.02271294988512551, 54.49948385550240459, 7.000000000000000888 ) ) ;
#9663 = DIRECTION ( 'NONE',  ( 9.710251638871371392E-17, 5.969973981896233748E-17, 1.000000000000000000 ) ) ;
#9664 = EDGE_LOOP ( 'NONE', ( #2309, #7434 ) ) ;
#9665 = ORIENTED_EDGE ( 'NONE', *, *, #7997, .F. ) ;
#9666 = CARTESIAN_POINT ( 'NONE',  ( 6.367873360227558344, 5.773502691896261751, 0.000000000000000000 ) ) ;
#9667 = ORIENTED_EDGE ( 'NONE', *, *, #16660, .F. ) ;
#9668 = CARTESIAN_POINT ( 'NONE',  ( 56.66441430157294690, 62.90051614449765083, -2.141517661632166281 ) ) ;
#9669 = EDGE_LOOP ( 'NONE', ( #5945, #4454, #2344, #18977, #12980, #3809, #17928, #18242, #3089, #17234, #4774, #18286, #11446, #7219, #11544, #17429 ) ) ;
#9670 = AXIS2_PLACEMENT_3D ( 'NONE', #11715, #17822, #10151 ) ;
#9671 = AXIS2_PLACEMENT_3D ( 'NONE', #1320, #17607, #11882 ) ;
#9672 = CARTESIAN_POINT ( 'NONE',  ( 45.90387839640214196, 46.69948385550240744, 5.676469297603166098 ) ) ;
#9673 = DIRECTION ( 'NONE',  ( -0.000000000000000000, -0.000000000000000000, -1.000000000000000000 ) ) ;
#9674 = CARTESIAN_POINT ( 'NONE',  ( 44.30067958973594955, 64.10051614449766078, -1.875703265242155693 ) ) ;
#9675 = LINE ( 'NONE', #6941, #18016 ) ;
#9676 = ADVANCED_FACE ( 'NONE', ( #2851 ), #11549, .F. ) ;
#9677 = DIRECTION ( 'NONE',  ( 1.000000000000000000, 0.000000000000000000, 0.000000000000000000 ) ) ;
#9678 = AXIS2_PLACEMENT_3D ( 'NONE', #3797, #11514, #6721 ) ;
#9679 = CARTESIAN_POINT ( 'NONE',  ( -19.02113032590304442, -26.18033988749903074, 9.000000000000000000 ) ) ;
#9680 = CARTESIAN_POINT ( 'NONE',  ( 42.39856655714564226, 58.10051614449765367, -2.493737253992044156 ) ) ;
#9681 = EDGE_CURVE ( 'NONE', #440, #10132, #14395, .T. ) ;
#9682 = ORIENTED_EDGE ( 'NONE', *, *, #13455, .F. ) ;
#9683 = VERTEX_POINT ( 'NONE', #12836 ) ;
#9684 = DIRECTION ( 'NONE',  ( 1.000000000000000000, 0.000000000000000000, 0.000000000000000000 ) ) ;
#9685 = SURFACE_SIDE_STYLE ('',( #777 ) ) ;
#9686 = AXIS2_PLACEMENT_3D ( 'NONE', #17001, #15510, #2085 ) ;
#9687 = DIRECTION ( 'NONE',  ( 0.000000000000000000, 0.000000000000000000, 1.000000000000000000 ) ) ;
#9688 = CONTEXT_DEPENDENT_SHAPE_REPRESENTATION ( #12660, #2593 ) ;
#9689 = ORIENTED_EDGE ( 'NONE', *, *, #7836, .T. ) ;
#9690 = DIRECTION ( 'NONE',  ( 0.8090169943749464521, 0.5877852522924744694, 0.000000000000000000 ) ) ;
#9691 = FACE_BOUND ( 'NONE', #11497, .T. ) ;
#9692 = AXIS2_PLACEMENT_3D ( 'NONE', #13856, #8066, #18593 ) ;
#9693 = VERTEX_POINT ( 'NONE', #7249 ) ;
#9694 = DIRECTION ( 'NONE',  ( 0.000000000000000000, 0.000000000000000000, 1.000000000000000000 ) ) ;
#9695 = CARTESIAN_POINT ( 'NONE',  ( -2.807080416178626692, 3.225969019225154444, -3.502507215260441065 ) ) ;
#9696 = CYLINDRICAL_SURFACE ( 'NONE', #7365, 10.00000000000000888 ) ;
#9697 = CONICAL_SURFACE ( 'NONE', #18189, 5.000000000000000000, 1.047197551196600296 ) ;
#9698 = LINE ( 'NONE', #8426, #12037 ) ;
#9699 = CARTESIAN_POINT ( 'NONE',  ( 4.165266963751721896, 2.049631966911991565, 3.550066703508901078 ) ) ;
#9700 = CARTESIAN_POINT ( 'NONE',  ( 44.30067958973596376, 46.89948385550240317, 1.875703265242204099 ) ) ;
#9701 = AXIS2_PLACEMENT_3D ( 'NONE', #2055, #11146, #15288 ) ;
#9702 = CARTESIAN_POINT ( 'NONE',  ( 4.071447262713887127, -2.020725942163686284, 3.500000000000000444 ) ) ;
#9703 = CARTESIAN_POINT ( 'NONE',  ( 54.68390685589033495, 63.69948385550240033, -6.485486291978119766 ) ) ;
#9704 = CARTESIAN_POINT ( 'NONE',  ( 43.34962307344078880, 64.10051614449766078, -2.184720259617096705 ) ) ;
#9705 = CARTESIAN_POINT ( 'NONE',  ( -2.321707774797442170, -4.824281976789052351, 0.000000000000000000 ) ) ;
#9706 = CARTESIAN_POINT ( 'NONE',  ( 6.507056315241514177, 2.833450876375910976, -5.092319121366348789 ) ) ;
#9707 = CARTESIAN_POINT ( 'NONE',  ( 0.000000000000000000, 15.00000000000001599, 20.60000000000000142 ) ) ;
#9708 = ORIENTED_EDGE ( 'NONE', *, *, #11929, .T. ) ;
#9709 = VECTOR ( 'NONE', #7938, 1000.000000000000000 ) ;
#9710 = LINE ( 'NONE', #6776, #6407 ) ;
#9711 = LINE ( 'NONE', #3746, #13142 ) ;
#9712 = VECTOR ( 'NONE', #12508, 1000.000000000000000 ) ;
#9713 = AXIS2_PLACEMENT_3D ( 'NONE', #6026, #19191, #12087 ) ;
#9714 = CARTESIAN_POINT ( 'NONE',  ( 54.13287192849671214, 54.70051614449766220, -5.649768623646139964 ) ) ;
#9715 = CARTESIAN_POINT ( 'NONE',  ( 54.56344682779376143, 44.99999999999996447, -5.899875555194201482 ) ) ;
#9716 = COLOUR_RGB ( '',0.8941176470588234615, 0.8941176470588234615, 0.8941176470588234615 ) ;
#9717 = DIRECTION ( 'NONE',  ( -0.000000000000000000, -0.000000000000000000, -1.000000000000000000 ) ) ;
#9718 = ORIENTED_EDGE ( 'NONE', *, *, #6027, .T. ) ;
#9719 = DIRECTION ( 'NONE',  ( -0.9781476007338065770, 0.2079116908177552348, 0.000000000000000000 ) ) ;
#9720 = DIRECTION ( 'NONE',  ( 1.000000000000000000, 0.000000000000000000, 0.000000000000000000 ) ) ;
#9721 = EDGE_CURVE ( 'NONE', #14983, #12007, #10272, .T. ) ;
#9722 = CARTESIAN_POINT ( 'NONE',  ( 20.00000000000000000, -25.00000000000000711, -20.00000000000000000 ) ) ;
#9723 = DIRECTION ( 'NONE',  ( -0.000000000000000000, 1.000000000000000000, 1.224646799147353207E-16 ) ) ;
#9724 = CARTESIAN_POINT ( 'NONE',  ( -154.9999999999999716, -14.99999999999999645, 3.999999999999999112 ) ) ;
#9725 = CARTESIAN_POINT ( 'NONE',  ( 45.27934281921082516, 57.70051614449766930, 6.458785618021089192 ) ) ;
#9726 = PRODUCT_DEFINITION ( 'UNKNOWN', '', #5102, #8719 ) ;
#9727 = CARTESIAN_POINT ( 'NONE',  ( 55.71335778527780036, 62.90051614449765083, -1.832500667257213056 ) ) ;
#9728 = DIRECTION ( 'NONE',  ( 1.000000000000000000, 0.000000000000000000, 0.000000000000000000 ) ) ;
#9729 = TOROIDAL_SURFACE ( 'NONE', #13187, 4.100000000000000533, 0.1000000000000001582 ) ;
#9730 = DIRECTION ( 'NONE',  ( 0.000000000000000000, 0.000000000000000000, 1.000000000000000000 ) ) ;
#9731 = CIRCLE ( 'NONE', #16651, 4.000000000000003553 ) ;
#9732 = VERTEX_POINT ( 'NONE', #16082 ) ;
#9733 = ORIENTED_EDGE ( 'NONE', *, *, #17186, .T. ) ;
#9734 = ORIENTED_EDGE ( 'NONE', *, *, #16598, .F. ) ;
#9735 = CARTESIAN_POINT ( 'NONE',  ( -0.9999999999999976685, -20.00000000000000000, 8.999999999999998224 ) ) ;
#9736 = EDGE_LOOP ( 'NONE', ( #7190, #8794 ) ) ;
#9737 = ADVANCED_FACE ( 'NONE', ( #9980 ), #16074, .F. ) ;
#9738 = CARTESIAN_POINT ( 'NONE',  ( -74.99999999999997158, -23.00000000000000355, -10.00000000000000178 ) ) ;
#9739 = EDGE_CURVE ( 'NONE', #9923, #4769, #12066, .T. ) ;
#9740 = EDGE_LOOP ( 'NONE', ( #18838, #12466, #16635, #15962 ) ) ;
#9741 = CARTESIAN_POINT ( 'NONE',  ( 2.449293598294706513E-15, -20.00000000000000000, 9.000000000000000000 ) ) ;
#9742 = CARTESIAN_POINT ( 'NONE',  ( 44.05948171654949874, 56.79948385550239465, 4.345558710429104465 ) ) ;
#9743 = VERTEX_POINT ( 'NONE', #7340 ) ;
#9744 = CARTESIAN_POINT ( 'NONE',  ( -1.317756351988340180, 3.857995168970202116, -0.04852650426601388955 ) ) ;
#9745 = ORIENTED_EDGE ( 'NONE', *, *, #6410, .F. ) ;
#9746 = CARTESIAN_POINT ( 'NONE',  ( 54.72065718078924590, 52.29948385550240886, 6.458785618021043895 ) ) ;
#9747 = AXIS2_PLACEMENT_3D ( 'NONE', #17279, #12846, #18855 ) ;
#9748 = DIRECTION ( 'NONE',  ( 0.000000000000000000, 0.000000000000000000, -1.000000000000000000 ) ) ;
#9749 = ADVANCED_FACE ( 'NONE', ( #6075 ), #12236, .T. ) ;
#9750 = PRODUCT_DEFINITION_SHAPE ( 'NONE', 'NONE',  #6612 ) ;
#9751 = CARTESIAN_POINT ( 'NONE',  ( 46.45491332379572924, 51.29948385550240175, -4.840751629271157874 ) ) ;
#9752 = CARTESIAN_POINT ( 'NONE',  ( 3.950241966888466738, 2.668221755853590782, 2.378504353001025695 ) ) ;
#9753 = PRESENTATION_LAYER_ASSIGNMENT (  '', '', ( #19185 ) ) ;
#9754 = ADVANCED_FACE ( 'NONE', ( #7723 ), #10664, .T. ) ;
#9755 = DIRECTION ( 'NONE',  ( 0.000000000000000000, 0.000000000000000000, 1.000000000000000000 ) ) ;
#9756 = CARTESIAN_POINT ( 'NONE',  ( 45.86712807150329496, 61.70051614449766220, 5.649768623646139964 ) ) ;
#9757 = CARTESIAN_POINT ( 'NONE',  ( 43.69122665457040000, 62.99948385550241170, 0.02388180880521036456 ) ) ;
#9758 = CARTESIAN_POINT ( 'NONE',  ( 55.94051828345050836, 59.79948385550238754, -4.345558710429104465 ) ) ;
#9759 = CARTESIAN_POINT ( 'NONE',  ( 3.861362476283255685, 2.629030857715988656, -3.671615880910370500 ) ) ;
#9760 = CARTESIAN_POINT ( 'NONE',  ( -5.130877905917149207, -39.33065161639853358, 0.000000000000000000 ) ) ;
#9761 = VERTEX_POINT ( 'NONE', #10562 ) ;
#9762 = EDGE_CURVE ( 'NONE', #2296, #828, #11762, .T. ) ;
#9763 = EDGE_CURVE ( 'NONE', #2420, #11339, #16784, .T. ) ;
#9764 = ORIENTED_EDGE ( 'NONE', *, *, #14194, .T. ) ;
#9765 = CARTESIAN_POINT ( 'NONE',  ( 0.000000000000000000, 0.000000000000000000, 0.000000000000000000 ) ) ;
#9766 = APPLICATION_PROTOCOL_DEFINITION ( 'draft international standard', 'automotive_design', 1998, #11246 ) ;
#9767 = EDGE_LOOP ( 'NONE', ( #12205, #5381, #9583, #16831 ) ) ;
#9768 = EDGE_CURVE ( 'NONE', #18532, #12297, #12710, .T. ) ;
#9769 = CARTESIAN_POINT ( 'NONE',  ( 45.90387839640214196, 56.69948385550240744, 5.676469297603166098 ) ) ;
#9770 = CARTESIAN_POINT ( 'NONE',  ( 2.482347295856823136E-15, -20.00000000000000000, -8.999999999999996447 ) ) ;
#9771 = ORIENTED_EDGE ( 'NONE', *, *, #79, .T. ) ;
#9772 = ORIENTED_EDGE ( 'NONE', *, *, #4420, .F. ) ;
#9773 = DIRECTION ( 'NONE',  ( 1.000000000000000000, 0.000000000000000000, 0.000000000000000000 ) ) ;
#9774 = VERTEX_POINT ( 'NONE', #9001 ) ;
#9775 = CARTESIAN_POINT ( 'NONE',  ( -57.64999999999994884, -14.99999999999998579, -10.00000000000000178 ) ) ;
#9776 = ORIENTED_EDGE ( 'NONE', *, *, #4974, .F. ) ;
#9777 = CARTESIAN_POINT ( 'NONE',  ( -74.99999999999997158, 20.00000000000001421, 15.00000000000000000 ) ) ;
#9778 = LINE ( 'NONE', #571, #2755 ) ;
#9779 = AXIS2_PLACEMENT_3D ( 'NONE', #18510, #14062, #8189 ) ;
#9780 = CARTESIAN_POINT ( 'NONE',  ( 51.97223112728249816, 60.60051614449765367, -5.992620115222793586 ) ) ;
#9781 = DIRECTION ( 'NONE',  ( -1.000000000000000000, 0.000000000000000000, 0.000000000000000000 ) ) ;
#9782 = CARTESIAN_POINT ( 'NONE',  ( -4.872650870659752442, 0.4273491293402474911, 0.000000000000000000 ) ) ;
#9783 = DIRECTION ( 'NONE',  ( 1.000000000000000000, 0.000000000000000000, 0.000000000000000000 ) ) ;
#9784 = ORIENTED_EDGE ( 'NONE', *, *, #13234, .T. ) ;
#9785 = VERTEX_POINT ( 'NONE', #4600 ) ;
#9786 = CARTESIAN_POINT ( 'NONE',  ( 4.000000000000000000, 0.8378280264232961239, -3.220590601395640018 ) ) ;
#9787 = SHAPE_REPRESENTATION_RELATIONSHIP ( 'NONE' , 'NONE' ,  #9916, #11988 ) ;
#9788 = DIRECTION ( 'NONE',  ( -2.191393683118470056E-17, -7.538405132783724027E-17, -1.000000000000000000 ) ) ;
#9789 = ORIENTED_EDGE ( 'NONE', *, *, #3244, .T. ) ;
#9790 = DIRECTION ( 'NONE',  ( -0.7779254092217071648, -0.6283566325640553840, 0.000000000000000000 ) ) ;
#9791 = EDGE_CURVE ( 'NONE', #6434, #7961, #198, .T. ) ;
#9792 = ORIENTED_EDGE ( 'NONE', *, *, #13722, .F. ) ;
#9793 = FILL_AREA_STYLE_COLOUR ( '', #11322 ) ;
#9794 = ADVANCED_FACE ( 'NONE', ( #14984 ), #9282, .F. ) ;
#9795 = DIRECTION ( 'NONE',  ( -1.000000000000000000, 0.000000000000000000, 0.000000000000000000 ) ) ;
#9796 = FACE_OUTER_BOUND ( 'NONE', #2464, .T. ) ;
#9797 = CARTESIAN_POINT ( 'NONE',  ( 32.49999999999998579, 40.00000000000001421, -4.999999999999996447 ) ) ;
#9798 = CARTESIAN_POINT ( 'NONE',  ( 4.132952817037859994, 2.031684012687258623, 3.518979934899746809 ) ) ;
#9799 = CARTESIAN_POINT ( 'NONE',  ( 44.28664221472220675, 49.09948385550241312, -1.832500667257165317 ) ) ;
#9800 = DIRECTION ( 'NONE',  ( 0.000000000000000000, 0.000000000000000000, 1.000000000000000000 ) ) ;
#9801 = CARTESIAN_POINT ( 'NONE',  ( 50.02271294988513972, 64.49948385550239038, 8.000000000000001776 ) ) ;
#9802 = CARTESIAN_POINT ( 'NONE',  ( 43.34962307344078880, 60.10051614449766078, -2.184720259617096705 ) ) ;
#9803 = DIRECTION ( 'NONE',  ( 0.000000000000000000, 0.000000000000000000, 1.000000000000000000 ) ) ;
#9804 = CARTESIAN_POINT ( 'NONE',  ( 6.541334219041337050, 2.934241909852039143, -5.143243597038033244 ) ) ;
#9805 = CARTESIAN_POINT ( 'NONE',  ( -62.49999999999997158, 32.50000000000001421, -20.00000000000000000 ) ) ;
#9806 = ORIENTED_EDGE ( 'NONE', *, *, #17782, .T. ) ;
#9807 = DIRECTION ( 'NONE',  ( 0.000000000000000000, 0.000000000000000000, 1.000000000000000000 ) ) ;
#9808 = FACE_BOUND ( 'NONE', #5780, .T. ) ;
#9809 = CARTESIAN_POINT ( 'NONE',  ( 43.33558569842706021, 51.90051614449765793, 2.141517661632167169 ) ) ;
#9810 = VECTOR ( 'NONE', #9530, 1000.000000000000000 ) ;
#9811 = CARTESIAN_POINT ( 'NONE',  ( 55.13865474201621453, 45.00000000000007816, -5.383573523308436748 ) ) ;
#9812 = CARTESIAN_POINT ( 'NONE',  ( 2.000000000000000000, 1.773042676681340524, -2.059984127722458425E-15 ) ) ;
#9813 = ORIENTED_EDGE ( 'NONE', *, *, #14844, .F. ) ;
#9814 = CARTESIAN_POINT ( 'NONE',  ( 4.055492966679659084, -3.795017426214758682, 0.5629142681442622642 ) ) ;
#9815 = CYLINDRICAL_SURFACE ( 'NONE', #4532, 9.999999999999998224 ) ;
#9816 = CARTESIAN_POINT ( 'NONE',  ( 75.00000000000001421, -7.499999999999971578, -10.00000000000000000 ) ) ;
#9817 = CARTESIAN_POINT ( 'NONE',  ( 56.66441430157296821, 46.09948385550240602, 2.141517661632100111 ) ) ;
#9818 = DIRECTION ( 'NONE',  ( -0.000000000000000000, -0.000000000000000000, 1.000000000000000000 ) ) ;
#9819 = CARTESIAN_POINT ( 'NONE',  ( 45.27934281921082516, 63.70051614449766930, 6.458785618021089192 ) ) ;
#9820 = DIRECTION ( 'NONE',  ( -1.000000000000000000, -0.000000000000000000, -0.000000000000000000 ) ) ;
#9821 = CARTESIAN_POINT ( 'NONE',  ( 56.30877334542961421, 61.00051614449765935, 0.02388180880515774693 ) ) ;
#9822 = CYLINDRICAL_SURFACE ( 'NONE', #16955, 1.000000000000000888 ) ;
#9823 = DIRECTION ( 'NONE',  ( -1.000000000000000000, 0.000000000000000000, 0.000000000000000000 ) ) ;
#9824 = AXIS2_PLACEMENT_3D ( 'NONE', #6195, #6101, #2883 ) ;
#9825 = ORIENTED_EDGE ( 'NONE', *, *, #766, .F. ) ;
#9826 = ORIENTED_EDGE ( 'NONE', *, *, #7525, .T. ) ;
#9827 = LINE ( 'NONE', #11307, #13749 ) ;
#9828 = ORIENTED_EDGE ( 'NONE', *, *, #7843, .T. ) ;
#9829 = DIRECTION ( 'NONE',  ( 0.000000000000000000, 0.000000000000000000, 1.000000000000000000 ) ) ;
#9830 = ORIENTED_EDGE ( 'NONE', *, *, #2105, .F. ) ;
#9831 = LINE ( 'NONE', #15832, #14094 ) ;
#9832 = CARTESIAN_POINT ( 'NONE',  ( 56.66441430157296821, 58.09948385550240602, 2.141517661632100111 ) ) ;
#9833 = VERTEX_POINT ( 'NONE', #1566 ) ;
#9834 = CARTESIAN_POINT ( 'NONE',  ( 9.999999999999994671, 20.00000000000001421, 9.999999999999998224 ) ) ;
#9835 = VERTEX_POINT ( 'NONE', #15090 ) ;
#9836 = CARTESIAN_POINT ( 'NONE',  ( 43.20883090819745576, 58.79948385550240175, 4.963592699179006473 ) ) ;
#9837 = CIRCLE ( 'NONE', #3600, 5.200000000000001066 ) ;
#9838 = CARTESIAN_POINT ( 'NONE',  ( -74.99999999999997158, -23.00000000000000355, 10.00000000000000000 ) ) ;
#9839 = CARTESIAN_POINT ( 'NONE',  ( 55.71335778527780747, 52.09948385550241312, 1.832500667257165983 ) ) ;
#9840 = CARTESIAN_POINT ( 'NONE',  ( 45.60000000000000142, 2.516649172247811061E-16, -2.055000000000000160 ) ) ;
#9841 = FACE_OUTER_BOUND ( 'NONE', #9634, .T. ) ;
#9842 = CARTESIAN_POINT ( 'NONE',  ( 42.38452918213190657, 45.90051614449766504, 2.450534656007115508 ) ) ;
#9843 = CARTESIAN_POINT ( 'NONE',  ( 49.97728705011488870, 63.49948385550241170, -6.000000000000000888 ) ) ;
#9844 = EDGE_CURVE ( 'NONE', #13265, #1140, #13609, .T. ) ;
#9845 = DIRECTION ( 'NONE',  ( -1.000000000000000000, -0.000000000000000000, -0.000000000000000000 ) ) ;
#9846 = FACE_OUTER_BOUND ( 'NONE', #3301, .T. ) ;
#9847 = ORIENTED_EDGE ( 'NONE', *, *, #6288, .T. ) ;
#9848 = VECTOR ( 'NONE', #2172, 1000.000000000000000 ) ;
#9849 = ORIENTED_EDGE ( 'NONE', *, *, #3404, .T. ) ;
#9850 = CARTESIAN_POINT ( 'NONE',  ( 62.50000000000000000, 32.50000000000001421, -15.00000000000000000 ) ) ;
#9851 =( NAMED_UNIT ( * ) SI_UNIT ( $, .STERADIAN. ) SOLID_ANGLE_UNIT ( ) );
#9852 = VERTEX_POINT ( 'NONE', #19335 ) ;
#9853 = VECTOR ( 'NONE', #4497, 1000.000000000000000 ) ;
#9854 = EDGE_CURVE ( 'NONE', #2618, #7151, #3014, .T. ) ;
#9855 = B_SPLINE_CURVE_WITH_KNOTS ( 'NONE', 3,
 ( #2844, #17946, #8808, #14782, #4504, #17842, #4480, #4402 ),
 .UNSPECIFIED., .F., .F.,
 ( 4, 2, 2, 4 ),
 ( 2.465131517390770070E-07, 0.001183067374689869946, 0.001774477805458935659, 0.002365888236228001588 ),
 .UNSPECIFIED. ) ;
#9856 = CARTESIAN_POINT ( 'NONE',  ( 49.97728705011488159, 59.49948385550240459, -7.000000000000000888 ) ) ;
#9857 = EDGE_CURVE ( 'NONE', #848, #6664, #17244, .T. ) ;
#9858 = CARTESIAN_POINT ( 'NONE',  ( -20.00000000000000000, -19.99999999999999289, -12.00000000000000000 ) ) ;
#9859 = ORIENTED_EDGE ( 'NONE', *, *, #10821, .F. ) ;
#9860 = EDGE_LOOP ( 'NONE', ( #13002, #3780, #633, #1104 ) ) ;
#9861 = CARTESIAN_POINT ( 'NONE',  ( 2.449293598294706513E-15, -20.00000000000000000, -50.00000000000000000 ) ) ;
#9862 = AXIS2_PLACEMENT_3D ( 'NONE', #7652, #4628, #16782 ) ;
#9863 = EDGE_CURVE ( 'NONE', #11041, #7511, #494, .T. ) ;
#9864 = ORIENTED_EDGE ( 'NONE', *, *, #320, .F. ) ;
#9865 = DIRECTION ( 'NONE',  ( 0.000000000000000000, 0.000000000000000000, -1.000000000000000000 ) ) ;
#9866 = VERTEX_POINT ( 'NONE', #4408 ) ;
#9867 = EDGE_CURVE ( 'NONE', #3997, #3999, #10376, .T. ) ;
#9868 = EDGE_CURVE ( 'NONE', #3752, #11744, #1441, .T. ) ;
#9869 = CARTESIAN_POINT ( 'NONE',  ( 50.02271294988512551, 50.49948385550240459, 7.000000000000000888 ) ) ;
#9870 = CARTESIAN_POINT ( 'NONE',  ( -11.75570504584937481, -36.18033988749900942, -9.000000000000000000 ) ) ;
#9871 = CARTESIAN_POINT ( 'NONE',  ( 55.71335778527780036, 62.90051614449765083, -1.832500667257213056 ) ) ;
#9872 = DIRECTION ( 'NONE',  ( 9.710251638871371392E-17, 5.969973981896233748E-17, 1.000000000000000000 ) ) ;
#9873 = CARTESIAN_POINT ( 'NONE',  ( 2.449293598294706513E-15, -20.00000000000000000, -9.000000000000000000 ) ) ;
#9874 = AXIS2_PLACEMENT_3D ( 'NONE', #3139, #3234, #9103 ) ;
#9875 = VERTEX_POINT ( 'NONE', #8207 ) ;
#9876 = ORIENTED_EDGE ( 'NONE', *, *, #14553, .T. ) ;
#9877 = LINE ( 'NONE', #11447, #18134 ) ;
#9878 = SHAPE_REPRESENTATION_RELATIONSHIP ( 'NONE' , 'NONE' ,  #1926, #780 ) ;
#9879 = ADVANCED_FACE ( 'NONE', ( #469 ), #13800, .T. ) ;
#9880 = CARTESIAN_POINT ( 'NONE',  ( -74.99999999999997158, -14.99999999999998934, 10.00000000000000000 ) ) ;
#9881 = AXIS2_PLACEMENT_3D ( 'NONE', #1066, #5173, #17152 ) ;
#9882 = EDGE_CURVE ( 'NONE', #9274, #3703, #5774, .T. ) ;
#9883 = CARTESIAN_POINT ( 'NONE',  ( 20.00000000000000000, -25.00000000000000711, -23.00000000000000000 ) ) ;
#9884 = ORIENTED_EDGE ( 'NONE', *, *, #320, .T. ) ;
#9885 = DIRECTION ( 'NONE',  ( -0.000000000000000000, -0.000000000000000000, 1.000000000000000000 ) ) ;
#9886 = EDGE_LOOP ( 'NONE', ( #18782, #16370, #13693, #1341 ) ) ;
#9887 = AXIS2_PLACEMENT_3D ( 'NONE', #9861, #17638, #9773 ) ;
#9888 = CARTESIAN_POINT ( 'NONE',  ( -16.32050807568879236, -10.00000000000004263, -9.000000000000000000 ) ) ;
#9889 = CARTESIAN_POINT ( 'NONE',  ( 4.142654963991853734, 4.070796997468700162, 1.458723597913840680E-15 ) ) ;
#9890 = CARTESIAN_POINT ( 'NONE',  ( 55.71335778527780747, 64.09948385550239891, 1.832500667257165983 ) ) ;
#9891 = CARTESIAN_POINT ( 'NONE',  ( -74.99999999999997158, 20.00000000000001421, -15.00000000000000000 ) ) ;
#9892 = CARTESIAN_POINT ( 'NONE',  ( 4.142654963991853734, 2.035398498734346973, 3.525413613457309747 ) ) ;
#9893 = CARTESIAN_POINT ( 'NONE',  ( 55.11794222512601493, 50.19948385550241454, 3.688883143319541702 ) ) ;
#9894 = CARTESIAN_POINT ( 'NONE',  ( 4.071447262713890680, -4.041451884327386779, 0.000000000000000000 ) ) ;
#9895 = CARTESIAN_POINT ( 'NONE',  ( 45.86712807150323812, 49.29948385550240175, -5.649768623646098220 ) ) ;
#9896 = CARTESIAN_POINT ( 'NONE',  ( 57.60143344285435774, 45.10051614449766788, 2.493737253992045044 ) ) ;
#9897 = DIRECTION ( 'NONE',  ( 0.000000000000000000, 0.000000000000000000, 1.000000000000000000 ) ) ;
#9898 = CARTESIAN_POINT ( 'NONE',  ( -4.999999999999998224, -20.00000000000000000, 9.999999999999998224 ) ) ;
#9899 = DIRECTION ( 'NONE',  ( 0.000000000000000000, 0.000000000000000000, 1.000000000000000000 ) ) ;
#9900 = ADVANCED_FACE ( 'NONE', ( #17242 ), #15563, .F. ) ;
#9901 = ORIENTED_EDGE ( 'NONE', *, *, #9480, .T. ) ;
#9902 = FACE_OUTER_BOUND ( 'NONE', #9250, .T. ) ;
#9903 = PRODUCT_DEFINITION_SHAPE ( 'NONE', 'NONE',  #19417 ) ;
#9904 = EDGE_CURVE ( 'NONE', #2618, #6141, #9377, .T. ) ;
#9905 = DIRECTION ( 'NONE',  ( -1.000000000000000000, 0.000000000000000000, 0.000000000000000000 ) ) ;
#9906 = CARTESIAN_POINT ( 'NONE',  ( 43.33558569842706021, 55.90051614449765793, 2.141517661632167169 ) ) ;
#9907 = AXIS2_PLACEMENT_3D ( 'NONE', #16224, #18093, #19288 ) ;
#9908 = CARTESIAN_POINT ( 'NONE',  ( 4.175075985190095373, -2.060370777630118777, 3.568666869285566090 ) ) ;
#9909 = DIRECTION ( 'NONE',  ( 0.000000000000000000, 0.000000000000000000, 1.000000000000000000 ) ) ;
#9910 = ORIENTED_EDGE ( 'NONE', *, *, #1141, .F. ) ;
#9911 = CARTESIAN_POINT ( 'NONE',  ( 3.974175853610083742, -3.450041667725777472, 1.156004144284040303 ) ) ;
#9912 = AXIS2_PLACEMENT_3D ( 'NONE', #8700, #7135, #13113 ) ;
#9913 = CARTESIAN_POINT ( 'NONE',  ( -74.99999999999997158, -6.999999999999989342, 15.00000000000000000 ) ) ;
#9914 = CARTESIAN_POINT ( 'NONE',  ( 4.140404888673277384, 2.228338276487440428, -3.686887068327033390 ) ) ;
#9915 = CARTESIAN_POINT ( 'NONE',  ( 55.94051828345050836, 49.79948385550240175, -4.345558710429104465 ) ) ;
#9916 = SHAPE_REPRESENTATION ( 'driver roller', ( #10359 ), #14982 ) ;
#9917 = DIRECTION ( 'NONE',  ( 0.000000000000000000, 0.000000000000000000, 1.000000000000000000 ) ) ;
#9918 = CARTESIAN_POINT ( 'NONE',  ( 43.18075615816989199, 49.19948385550240744, -4.924951120819313743 ) ) ;
#9919 = DIRECTION ( 'NONE',  ( -0.000000000000000000, -0.000000000000000000, -1.000000000000000000 ) ) ;
#9920 = CARTESIAN_POINT ( 'NONE',  ( 55.94051828345053679, 51.20051614449766220, 4.345558710429044069 ) ) ;
#9921 = EDGE_CURVE ( 'NONE', #15831, #1750, #12617, .T. ) ;
#9922 = CARTESIAN_POINT ( 'NONE',  ( -74.99999999999997158, 45.00000000000001421, 15.00000000000000000 ) ) ;
#9923 = VERTEX_POINT ( 'NONE', #9666 ) ;
#9924 = ADVANCED_FACE ( 'NONE', ( #385 ), #18624, .T. ) ;
#9925 = CIRCLE ( 'NONE', #9610, 0.7500000000000000000 ) ;
#9926 = EDGE_LOOP ( 'NONE', ( #14832, #10032, #14710 ) ) ;
#9927 = FACE_OUTER_BOUND ( 'NONE', #17723, .T. ) ;
#9928 = ORIENTED_EDGE ( 'NONE', *, *, #12262, .T. ) ;
#9929 = CARTESIAN_POINT ( 'NONE',  ( 4.180231680468789790, -2.085385483809538698, 3.570466434508605680 ) ) ;
#9930 = VERTEX_POINT ( 'NONE', #13977 ) ;
#9931 = FACE_OUTER_BOUND ( 'NONE', #14149, .T. ) ;
#9932 = CARTESIAN_POINT ( 'NONE',  ( 56.66441430157296821, 56.09948385550240602, 2.141517661632100111 ) ) ;
#9933 = EDGE_LOOP ( 'NONE', ( #4211, #8990, #5628, #14239 ) ) ;
#9934 = CARTESIAN_POINT ( 'NONE',  ( -31.74999999999995737, 0.000000000000000000, 2.000000000000000888 ) ) ;
#9935 = ORIENTED_EDGE ( 'NONE', *, *, #2217, .T. ) ;
#9936 = VECTOR ( 'NONE', #6570, 1000.000000000000000 ) ;
#9937 = CARTESIAN_POINT ( 'NONE',  ( 45.31609314410967926, 56.69948385550240744, 6.485486291978119766 ) ) ;
#9938 = DIRECTION ( 'NONE',  ( -1.000000000000000000, 0.000000000000000000, 0.000000000000000000 ) ) ;
#9939 = CIRCLE ( 'NONE', #10879, 20.00000000000000000 ) ;
#9940 = CARTESIAN_POINT ( 'NONE',  ( 55.69932041026404335, 53.89948385550240317, -1.875703265242203432 ) ) ;
#9941 = FACE_OUTER_BOUND ( 'NONE', #11396, .T. ) ;
#9942 = DIRECTION ( 'NONE',  ( 0.000000000000000000, 0.000000000000000000, 1.000000000000000000 ) ) ;
#9943 = CARTESIAN_POINT ( 'NONE',  ( 58.41169779390614281, 47.00051614449766646, 0.02388180880515032231 ) ) ;
#9944 = CARTESIAN_POINT ( 'NONE',  ( 43.69122665457040000, 64.99948385550240459, 0.02388180880521036456 ) ) ;
#9945 = CARTESIAN_POINT ( 'NONE',  ( -52.34999999999998010, -14.99999999999998579, -10.00000000000000178 ) ) ;
#9946 = CARTESIAN_POINT ( 'NONE',  ( -14.14213562373094746, -25.00000000000000000, -23.00000000000000000 ) ) ;
#9947 = ORIENTED_EDGE ( 'NONE', *, *, #18277, .F. ) ;
#9948 = VERTEX_POINT ( 'NONE', #3705 ) ;
#9949 = DIRECTION ( 'NONE',  ( -1.000000000000000000, 0.000000000000000000, 0.000000000000000000 ) ) ;
#9950 = ORIENTED_EDGE ( 'NONE', *, *, #14474, .T. ) ;
#9951 = AXIS2_PLACEMENT_3D ( 'NONE', #17360, #11945, #17845 ) ;
#9952 = AXIS2_PLACEMENT_3D ( 'NONE', #19031, #11151, #977 ) ;
#9953 = CARTESIAN_POINT ( 'NONE',  ( 52.25172492374522903, 55.59948385550241312, -7.007379884777225953 ) ) ;
#9954 = CARTESIAN_POINT ( 'NONE',  ( -1.000000000000000222, -4.808326913195983821, -0.8000000000000000444 ) ) ;
#9955 = ORIENTED_EDGE ( 'NONE', *, *, #7093, .F. ) ;
#9956 = ORIENTED_EDGE ( 'NONE', *, *, #6215, .T. ) ;
#9957 = DIRECTION ( 'NONE',  ( 0.000000000000000000, -0.000000000000000000, 1.000000000000000000 ) ) ;
#9958 = ORIENTED_EDGE ( 'NONE', *, *, #12641, .T. ) ;
#9959 = DIRECTION ( 'NONE',  ( 0.000000000000000000, 0.000000000000000000, 1.000000000000000000 ) ) ;
#9960 = ORIENTED_EDGE ( 'NONE', *, *, #8736, .T. ) ;
#9961 = CARTESIAN_POINT ( 'NONE',  ( 55.94051828345050836, 51.79948385550240175, -4.345558710429104465 ) ) ;
#9962 = DIRECTION ( 'NONE',  ( -0.9768494444668812671, -0.2139279384389642935, 0.000000000000000000 ) ) ;
#9963 = CARTESIAN_POINT ( 'NONE',  ( 47.74827507625469281, 48.40051614449764372, -7.007379884777203749 ) ) ;
#9964 = DIRECTION ( 'NONE',  ( 0.000000000000000000, 1.000000000000000000, 0.000000000000000000 ) ) ;
#9965 = EDGE_CURVE ( 'NONE', #13867, #2874, #3320, .T. ) ;
#9966 = CONICAL_SURFACE ( 'NONE', #13740, 1.535500000000000087, 1.047197551196590748 ) ;
#9967 = LINE ( 'NONE', #15969, #17095 ) ;
#9968 = CARTESIAN_POINT ( 'NONE',  ( -0.4472135954999577612, 5.633375276077824112E-16, 4.599999999999999645 ) ) ;
#9969 = EDGE_CURVE ( 'NONE', #14655, #17840, #18533, .T. ) ;
#9970 = STYLED_ITEM ( 'NONE', ( #9278 ), #6165 ) ;
#9971 = ORIENTED_EDGE ( 'NONE', *, *, #5482, .T. ) ;
#9972 = ORIENTED_EDGE ( 'NONE', *, *, #14784, .F. ) ;
#9973 = CARTESIAN_POINT ( 'NONE',  ( -2.500000000000000888, 0.000000000000000000, -4.974599999999998801 ) ) ;
#9974 =( NAMED_UNIT ( * ) PLANE_ANGLE_UNIT ( ) SI_UNIT ( $, .RADIAN. ) );
#9975 = ADVANCED_FACE ( 'NONE', ( #15463 ), #15274, .T. ) ;
#9976 = EDGE_CURVE ( 'NONE', #1555, #2510, #12329, .T. ) ;
#9977 = DIRECTION ( 'NONE',  ( 0.000000000000000000, 0.000000000000000000, -1.000000000000000000 ) ) ;
#9978 = CONTEXT_DEPENDENT_SHAPE_REPRESENTATION ( #16431, #3975 ) ;
#9979 = ORIENTED_EDGE ( 'NONE', *, *, #8177, .T. ) ;
#9980 = FACE_OUTER_BOUND ( 'NONE', #2754, .T. ) ;
#9981 = VECTOR ( 'NONE', #9449, 1000.000000000000000 ) ;
#9982 = ADVANCED_FACE ( 'NONE', ( #4973 ), #12381, .T. ) ;
#9983 = ORIENTED_EDGE ( 'NONE', *, *, #16132, .T. ) ;
#9984 = EDGE_LOOP ( 'NONE', ( #14265, #2343, #16540, #11598 ) ) ;
#9985 = LINE ( 'NONE', #14793, #14091 ) ;
#9986 = AXIS2_PLACEMENT_3D ( 'NONE', #9805, #14316, #6866 ) ;
#9987 = CARTESIAN_POINT ( 'NONE',  ( 0.03027795056225670092, 0.6888063905605149584, -3.499999999999999556 ) ) ;
#9988 = CARTESIAN_POINT ( 'NONE',  ( 55.08986747509849380, 51.20051614449766220, 3.727524721679155384 ) ) ;
#9989 = DIRECTION ( 'NONE',  ( 0.1305261922200521840, -0.9914448613738103822, 0.000000000000000000 ) ) ;
#9990 = EDGE_CURVE ( 'NONE', #8706, #9638, #18718, .T. ) ;
#9991 = CARTESIAN_POINT ( 'NONE',  ( -31.74999999999995737, 0.000000000000000000, 0.000000000000000000 ) ) ;
#9992 = EDGE_CURVE ( 'NONE', #10178, #1337, #5187, .T. ) ;
#9993 = CARTESIAN_POINT ( 'NONE',  ( 44.30067958973596376, 48.89948385550241028, 1.875703265242204099 ) ) ;
#9994 = CARTESIAN_POINT ( 'NONE',  ( 0.000000000000000000, -3.031088913245531202, 1.750000000000006439 ) ) ;
#9995 = CARTESIAN_POINT ( 'NONE',  ( 47.74827507625478518, 46.59948385550239891, 7.007379884777227730 ) ) ;
#9996 = CIRCLE ( 'NONE', #4992, 2.149999999999999023 ) ;
#9997 = CARTESIAN_POINT ( 'NONE',  ( 43.20883090819742023, 46.20051614449766220, -4.963592699178938972 ) ) ;
#9998 = AXIS2_PLACEMENT_3D ( 'NONE', #14532, #8754, #17790 ) ;
#9999 = LINE ( 'NONE', #19156, #12829 ) ;
#10000 = LINE ( 'NONE', #12945, #4315 ) ;
#10001 =( LENGTH_UNIT ( ) NAMED_UNIT ( * ) SI_UNIT ( .MILLI., .METRE. ) );
#10002 = DIRECTION ( 'NONE',  ( -1.000000000000000000, 0.000000000000000000, 6.123233995736766036E-17 ) ) ;
#10003 = AXIS2_PLACEMENT_3D ( 'NONE', #3189, #7675, #10712 ) ;
#10004 = ORIENTED_EDGE ( 'NONE', *, *, #17118, .F. ) ;
#10005 = CARTESIAN_POINT ( 'NONE',  ( 3.333333333333332593, 2.694301256218250007, -3.300726591567078483 ) ) ;
#10006 = CARTESIAN_POINT ( 'NONE',  ( -3.160591952521660364, -3.281206521718067037, 0.000000000000000000 ) ) ;
#10007 = CARTESIAN_POINT ( 'NONE',  ( 55.96859303347802239, 54.80051614449764941, -4.306917132069484566 ) ) ;
#10008 = AXIS2_PLACEMENT_3D ( 'NONE', #4909, #1883, #7850 ) ;
#10009 = LINE ( 'NONE', #11866, #7811 ) ;
#10010 = CARTESIAN_POINT ( 'NONE',  ( 2.449293598294706513E-15, -20.00000000000000000, 9.000000000000000000 ) ) ;
#10011 = ORIENTED_EDGE ( 'NONE', *, *, #16598, .T. ) ;
#10012 = CIRCLE ( 'NONE', #14084, 20.00000000000000000 ) ;
#10013 = DIRECTION ( 'NONE',  ( 0.000000000000000000, 0.000000000000000000, 1.000000000000000000 ) ) ;
#10014 = CARTESIAN_POINT ( 'NONE',  ( 3.453038570460273071, 2.625189405340834448, -3.535263753543585352 ) ) ;
#10015 = CARTESIAN_POINT ( 'NONE',  ( 42.63976443033212860, 52.99948385550240459, 0.02388180880522514787 ) ) ;
#10016 = AXIS2_PLACEMENT_3D ( 'NONE', #14752, #1336, #7310 ) ;
#10017 = DIRECTION ( 'NONE',  ( 0.000000000000000000, 0.000000000000000000, 1.000000000000000000 ) ) ;
#10018 = CARTESIAN_POINT ( 'NONE',  ( 57.61547081786812896, 46.09948385550240602, 2.450534656007040901 ) ) ;
#10019 = LINE ( 'NONE', #16209, #15711 ) ;
#10020 = CARTESIAN_POINT ( 'NONE',  ( 52.25172492374527877, 45.40051614449766504, 7.007379884777203749 ) ) ;
#10021 = CARTESIAN_POINT ( 'NONE',  ( 4.071447262713890680, -4.041451884327386779, 0.000000000000000000 ) ) ;
#10022 = APPLICATION_CONTEXT ( 'automotive_design' ) ;
#10023 = CARTESIAN_POINT ( 'NONE',  ( 6.212075932873402984, -2.040040303548923628, 4.999999999999999112 ) ) ;
#10024 = VECTOR ( 'NONE', #12552, 1000.000000000000000 ) ;
#10025 = ORIENTED_EDGE ( 'NONE', *, *, #8194, .F. ) ;
#10026 = AXIS2_PLACEMENT_3D ( 'NONE', #17824, #19310, #10345 ) ;
#10027 = ORIENTED_EDGE ( 'NONE', *, *, #6507, .T. ) ;
#10028 = DIRECTION ( 'NONE',  ( 1.000000000000000000, 0.000000000000000000, 0.000000000000000000 ) ) ;
#10029 = ORIENTED_EDGE ( 'NONE', *, *, #10347, .F. ) ;
#10030 = CARTESIAN_POINT ( 'NONE',  ( -154.9999999999999716, -14.99999999999999645, 17.00000000000000000 ) ) ;
#10031 = CIRCLE ( 'NONE', #1278, 1.000000000000000222 ) ;
#10032 = ORIENTED_EDGE ( 'NONE', *, *, #7478, .T. ) ;
#10033 = CARTESIAN_POINT ( 'NONE',  ( -164.9999999999999716, -14.99999999999999645, 4.000000000000000000 ) ) ;
#10034 = EDGE_CURVE ( 'NONE', #18478, #18720, #818, .T. ) ;
#10035 = ORIENTED_EDGE ( 'NONE', *, *, #11095, .F. ) ;
#10036 = DIRECTION ( 'NONE',  ( -1.000000000000000000, -0.000000000000000000, -0.000000000000000000 ) ) ;
#10037 = EDGE_LOOP ( 'NONE', ( #7024, #15755, #16509, #14469 ) ) ;
#10038 =( BOUNDED_SURFACE ( )  B_SPLINE_SURFACE ( 3, 2, ( 
 ( #16101, #19359, #11674 ),
 ( #1098, #2684, #5896 ),
 ( #8443, #7271, #8636 ),
 ( #14608, #14711, #14513 ),
 ( #16194, #13149, #17481 ),
 ( #4328, #4230, #16006 ) ),
 .UNSPECIFIED., .F., .F., .F. ) 
 B_SPLINE_SURFACE_WITH_KNOTS ( ( 4, 2, 4 ),
 ( 3, 3 ),
 ( 0.02032853247518126918, 0.02278863295364821906, 0.02524873343211516893 ),
 ( 0.000000000000000000, 1.000000000000000000 ),
 .UNSPECIFIED. ) 
 GEOMETRIC_REPRESENTATION_ITEM ( )  RATIONAL_B_SPLINE_SURFACE ( (
 ( 1.000000000000000000, 0.8047781615896838492, 1.000000000000000000),
 ( 1.000000000000000000, 0.8123767586288186404, 1.000000000000000000),
 ( 1.000000000000000000, 0.8190662415565814758, 1.000000000000000000),
 ( 1.000000000000000000, 0.8192361015667604107, 1.000000000000000000),
 ( 1.000000000000000000, 0.8126135807104967190, 1.000000000000000000),
 ( 1.000000000000000000, 0.8047712338318580017, 1.000000000000000000) ) ) 
 REPRESENTATION_ITEM ( '' )  SURFACE ( )  );
#10039 = CARTESIAN_POINT ( 'NONE',  ( 58.41169779390614281, 61.99948385550241170, -0.02388180880523160798 ) ) ;
#10040 = CIRCLE ( 'NONE', #9112, 2.000000000000001776 ) ;
#10041 = CARTESIAN_POINT ( 'NONE',  ( 0.000000000000000000, 0.000000000000000000, -4.484454397937119197 ) ) ;
#10042 = ADVANCED_FACE ( 'NONE', ( #7913 ), #2346, .T. ) ;
#10043 = CARTESIAN_POINT ( 'NONE',  ( 43.69122665457040000, 48.99948385550241170, 0.02388180880521036456 ) ) ;
#10044 = DIRECTION ( 'NONE',  ( 1.000000000000000000, 0.000000000000000000, 0.000000000000000000 ) ) ;
#10045 = DIRECTION ( 'NONE',  ( 0.000000000000000000, 0.000000000000000000, -1.000000000000000000 ) ) ;
#10046 = VECTOR ( 'NONE', #17146, 1000.000000000000000 ) ;
#10047 = AXIS2_PLACEMENT_3D ( 'NONE', #1526, #5743, #16531 ) ;
#10048 = CARTESIAN_POINT ( 'NONE',  ( 57.61547081786810764, 44.90051614449765793, -2.450534656007114176 ) ) ;
#10049 = CARTESIAN_POINT ( 'NONE',  ( 46.45491332379576477, 47.70051614449766220, 4.840751629271188961 ) ) ;
#10050 = CARTESIAN_POINT ( 'NONE',  ( 2.449848172108560096, 3.432307619358740514, -3.503702292528905637 ) ) ;
#10051 = CARTESIAN_POINT ( 'NONE',  ( 22.14999999999999858, -20.00000000000000000, -23.00000000000000000 ) ) ;
#10052 = ORIENTED_EDGE ( 'NONE', *, *, #11665, .F. ) ;
#10053 = VERTEX_POINT ( 'NONE', #15766 ) ;
#10054 = CARTESIAN_POINT ( 'NONE',  ( 2.321707774797442170, -4.824281976789052351, 0.000000000000000000 ) ) ;
#10055 = SURFACE_SIDE_STYLE ('',( #5543 ) ) ;
#10056 = ORIENTED_EDGE ( 'NONE', *, *, #2015, .T. ) ;
#10057 = CARTESIAN_POINT ( 'NONE',  ( 43.34962307344081012, 58.89948385550241028, 2.184720259617164650 ) ) ;
#10058 = DIRECTION ( 'NONE',  ( -0.000000000000000000, 1.000000000000000000, 0.000000000000000000 ) ) ;
#10059 = ORIENTED_EDGE ( 'NONE', *, *, #18347, .F. ) ;
#10060 = AXIS2_PLACEMENT_3D ( 'NONE', #12654, #18463, #13833 ) ;
#10061 = ORIENTED_EDGE ( 'NONE', *, *, #265, .F. ) ;
#10062 = DIRECTION ( 'NONE',  ( 0.000000000000000000, 0.000000000000000000, 1.000000000000000000 ) ) ;
#10063 = DIRECTION ( 'NONE',  ( -1.545477659731174253E-22, 3.805888647522192075E-23, -1.000000000000000000 ) ) ;
#10064 = AXIS2_PLACEMENT_3D ( 'NONE', #10934, #15259, #175 ) ;
#10065 = ORIENTED_EDGE ( 'NONE', *, *, #6993, .F. ) ;
#10066 = CARTESIAN_POINT ( 'NONE',  ( 4.197393957002303999, 7.772902908466098641E-14, -3.503767560748929810 ) ) ;
#10067 = ORIENTED_EDGE ( 'NONE', *, *, #13480, .T. ) ;
#10068 = DIRECTION ( 'NONE',  ( 1.000000000000000000, 0.000000000000000000, 0.000000000000000000 ) ) ;
#10069 = CARTESIAN_POINT ( 'NONE',  ( 43.34962307344081012, 50.89948385550241028, 2.184720259617164650 ) ) ;
#10070 = CARTESIAN_POINT ( 'NONE',  ( 18.68843350152500093, -27.12337372732038432, -9.000000000000000000 ) ) ;
#10071 = CARTESIAN_POINT ( 'NONE',  ( 44.05948171654945611, 50.20051614449764088, -4.345558710429044069 ) ) ;
#10072 = CARTESIAN_POINT ( 'NONE',  ( 45.60000000000000142, 0.000000000000000000, 2.055000000000000160 ) ) ;
#10073 = SURFACE_SIDE_STYLE ('',( #5466 ) ) ;
#10074 = DIRECTION ( 'NONE',  ( -0.3090169943749528914, 0.9510565162951518658, 0.000000000000000000 ) ) ;
#10075 = PRODUCT ( 'idle-roller mover', 'idle-roller mover', '', ( #16981 ) ) ;
#10076 = AXIS2_PLACEMENT_3D ( 'NONE', #13299, #15251, #7613 ) ;
#10077 = ORIENTED_EDGE ( 'NONE', *, *, #10935, .F. ) ;
#10078 = EDGE_LOOP ( 'NONE', ( #12793, #10911, #10539, #5342 ) ) ;
#10079 = CYLINDRICAL_SURFACE ( 'NONE', #17182, 0.9999999999999991118 ) ;
#10080 =( LENGTH_UNIT ( ) NAMED_UNIT ( * ) SI_UNIT ( .MILLI., .METRE. ) );
#10081 = DIRECTION ( 'NONE',  ( 0.000000000000000000, 0.000000000000000000, -1.000000000000000000 ) ) ;
#10082 = SURFACE_STYLE_FILL_AREA ( #16080 ) ;
#10083 = ORIENTED_EDGE ( 'NONE', *, *, #9030, .F. ) ;
#10084 = CARTESIAN_POINT ( 'NONE',  ( -1.250000000000001110, 6.827405905246494173E-16, 5.575000000000000178 ) ) ;
#10085 = ADVANCED_FACE ( 'NONE', ( #5753 ), #18917, .F. ) ;
#10086 = VECTOR ( 'NONE', #14847, 1000.000000000000000 ) ;
#10087 = VERTEX_POINT ( 'NONE', #11719 ) ;
#10088 = ORIENTED_EDGE ( 'NONE', *, *, #2710, .F. ) ;
#10089 = PRODUCT_DEFINITION ( 'UNKNOWN', '', #16398, #11655 ) ;
#10090 = DIRECTION ( 'NONE',  ( -0.000000000000000000, -0.000000000000000000, -1.000000000000000000 ) ) ;
#10091 = CARTESIAN_POINT ( 'NONE',  ( 4.158413352280809328, 4.089743253945647972, 1.634918261399485461E-15 ) ) ;
#10092 = CARTESIAN_POINT ( 'NONE',  ( 51.97223112728249816, 46.60051614449764656, -5.992620115222793586 ) ) ;
#10093 = DIRECTION ( 'NONE',  ( -0.000000000000000000, -0.000000000000000000, -1.000000000000000000 ) ) ;
#10094 = CARTESIAN_POINT ( 'NONE',  ( 4.158413352280808439, 2.044871626972822209, 3.541821552872961298 ) ) ;
#10095 = CARTESIAN_POINT ( 'NONE',  ( 55.69932041026404335, 53.89948385550240317, -1.875703265242203432 ) ) ;
#10096 = CARTESIAN_POINT ( 'NONE',  ( -1.959187206999195895E-15, 3.202582148906728765, 1.452965002680430828 ) ) ;
#10097 = CARTESIAN_POINT ( 'NONE',  ( 45.86712807150323812, 47.29948385550240886, -5.649768623646098220 ) ) ;
#10098 = CARTESIAN_POINT ( 'NONE',  ( 52.57664461997821093, 45.40051614449765793, 8.007379884777206414 ) ) ;
#10099 = CARTESIAN_POINT ( 'NONE',  ( 4.175075985190096262, -2.060370777630117889, -3.568666869285569643 ) ) ;
#10100 = EDGE_CURVE ( 'NONE', #18734, #12908, #10809, .T. ) ;
#10101 = DIRECTION ( 'NONE',  ( -0.000000000000000000, -0.000000000000000000, -1.000000000000000000 ) ) ;
#10102 = SHAPE_REPRESENTATION_RELATIONSHIP ( 'NONE' , 'NONE' ,  #19357, #5922 ) ;
#10103 = SHAPE_DEFINITION_REPRESENTATION ( #13356, #14681 ) ;
#10104 = VECTOR ( 'NONE', #7087, 1000.000000000000000 ) ;
#10105 = ORIENTED_EDGE ( 'NONE', *, *, #16414, .T. ) ;
#10106 = CARTESIAN_POINT ( 'NONE',  ( -15.51323935927273645, -7.377028694403556131, 0.000000000000000000 ) ) ;
#10107 = ADVANCED_FACE ( 'NONE', ( #19013 ), #8506, .T. ) ;
#10108 = ADVANCED_FACE ( 'NONE', ( #14272 ), #17535, .T. ) ;
#10109 = CARTESIAN_POINT ( 'NONE',  ( -29.99999999999999645, -40.00000000000000000, 10.00000000000000000 ) ) ;
#10110 = CARTESIAN_POINT ( 'NONE',  ( 6.355827204229362870, -3.436818823786764288, -4.264647808192651546 ) ) ;
#10111 = DIRECTION ( 'NONE',  ( 0.000000000000000000, 0.5000000000000011102, 0.8660254037844379305 ) ) ;
#10112 = CARTESIAN_POINT ( 'NONE',  ( 2.000000000000000000, -6.429618962271402616, -1.000000000000000000 ) ) ;
#10113 = CARTESIAN_POINT ( 'NONE',  ( 0.000000000000000000, 0.000000000000000000, 4.000000000000000000 ) ) ;
#10114 = EDGE_CURVE ( 'NONE', #4021, #14560, #8296, .T. ) ;
#10115 = CARTESIAN_POINT ( 'NONE',  ( 4.235886605889389145, 2.417314728048528760, -3.751161874094018245 ) ) ;
#10116 = CARTESIAN_POINT ( 'NONE',  ( 50.02271294988512551, 54.49948385550240459, 7.000000000000000888 ) ) ;
#10117 = CYLINDRICAL_SURFACE ( 'NONE', #132, 1.000000000000000888 ) ;
#10118 = CARTESIAN_POINT ( 'NONE',  ( 57.60143344285433642, 49.89948385550241028, -2.493737253992118319 ) ) ;
#10119 = CARTESIAN_POINT ( 'NONE',  ( -74.99999999999997158, -6.999999999999989342, -10.00000000000000178 ) ) ;
#10120 = CARTESIAN_POINT ( 'NONE',  ( 56.65037692655921120, 47.10051614449766078, 2.184720259617097593 ) ) ;
#10121 = CARTESIAN_POINT ( 'NONE',  ( 8.500000000000000000, 0.000000000000000000, 0.000000000000000000 ) ) ;
#10122 = VERTEX_POINT ( 'NONE', #856 ) ;
#10123 = VERTEX_POINT ( 'NONE', #1150 ) ;
#10124 = FACE_OUTER_BOUND ( 'NONE', #7085, .T. ) ;
#10125 = EDGE_LOOP ( 'NONE', ( #4905, #9972, #10707, #16727, #4178 ) ) ;
#10126 = EDGE_CURVE ( 'NONE', #2700, #5077, #5551, .T. ) ;
#10127 = CARTESIAN_POINT ( 'NONE',  ( 50.00000000000000000, 40.00000000000000000, -4.000000000000003553 ) ) ;
#10128 = ORIENTED_EDGE ( 'NONE', *, *, #2609, .T. ) ;
#10129 = CARTESIAN_POINT ( 'NONE',  ( 2.449293598294706513E-15, -20.00000000000000000, 9.000000000000000000 ) ) ;
#10130 = ORIENTED_EDGE ( 'NONE', *, *, #8738, .T. ) ;
#10131 = DIRECTION ( 'NONE',  ( -0.000000000000000000, -0.000000000000000000, -1.000000000000000000 ) ) ;
#10132 = VERTEX_POINT ( 'NONE', #2643 ) ;
#10133 = CARTESIAN_POINT ( 'NONE',  ( 45.31609314410967926, 58.69948385550240033, 6.485486291978119766 ) ) ;
#10134 = CARTESIAN_POINT ( 'NONE',  ( -0.2500000000000000000, -8.096141056083446585, -1.000000000000000000 ) ) ;
#10135 = CARTESIAN_POINT ( 'NONE',  ( 43.69122665457040000, 50.99948385550241170, 0.02388180880521036456 ) ) ;
#10136 = AXIS2_PLACEMENT_3D ( 'NONE', #1712, #1423, #3274 ) ;
#10137 = CARTESIAN_POINT ( 'NONE',  ( 0.000000000000000000, 1.773042676681340524, -2.059984127722458425E-15 ) ) ;
#10138 = CARTESIAN_POINT ( 'NONE',  ( 2.449293598294706513E-15, -20.00000000000000000, 9.000000000000000000 ) ) ;
#10139 = CARTESIAN_POINT ( 'NONE',  ( 54.68390685589039890, 49.30051614449766362, 6.485486291978072693 ) ) ;
#10140 = AXIS2_PLACEMENT_3D ( 'NONE', #1310, #4241, #11586 ) ;
#10141 = CARTESIAN_POINT ( 'NONE',  ( 51.92680522751238925, 47.40051614449765793, 6.007379884777208190 ) ) ;
#10142 = DIRECTION ( 'NONE',  ( 1.000000000000000000, 0.000000000000000000, -0.000000000000000000 ) ) ;
#10143 = CARTESIAN_POINT ( 'NONE',  ( -14.86289650954781649, -33.38261212717723936, -9.000000000000000000 ) ) ;
#10144 = VERTEX_POINT ( 'NONE', #17346 ) ;
#10145 = EDGE_CURVE ( 'NONE', #9447, #11744, #6830, .T. ) ;
#10146 = EDGE_LOOP ( 'NONE', ( #14399, #3411 ) ) ;
#10147 = DIRECTION ( 'NONE',  ( -1.000000000000000000, 0.000000000000000000, 0.000000000000000000 ) ) ;
#10148 = ORIENTED_EDGE ( 'NONE', *, *, #12522, .T. ) ;
#10149 = EDGE_CURVE ( 'NONE', #666, #9447, #7397, .T. ) ;
#10150 = CARTESIAN_POINT ( 'NONE',  ( 52.25172492374522903, 57.59948385550241312, -7.007379884777225953 ) ) ;
#10151 = DIRECTION ( 'NONE',  ( 1.000000000000000000, 0.000000000000000000, 0.000000000000000000 ) ) ;
#10152 = ORIENTED_EDGE ( 'NONE', *, *, #16523, .T. ) ;
#10153 = ORIENTED_EDGE ( 'NONE', *, *, #4727, .F. ) ;
#10154 = AXIS2_PLACEMENT_3D ( 'NONE', #12651, #10882, #6375 ) ;
#10155 = DIRECTION ( 'NONE',  ( 0.000000000000000000, 0.000000000000000000, 1.000000000000000000 ) ) ;
#10156 = CARTESIAN_POINT ( 'NONE',  ( -154.9999999999999716, -14.99999999999999645, -3.999999999999999112 ) ) ;
#10157 = ORIENTED_EDGE ( 'NONE', *, *, #17679, .T. ) ;
#10158 = DIRECTION ( 'NONE',  ( -1.000000000000000000, -0.000000000000000000, -0.000000000000000000 ) ) ;
#10159 = ORIENTED_EDGE ( 'NONE', *, *, #14534, .T. ) ;
#10160 = CARTESIAN_POINT ( 'NONE',  ( -154.9999999999999716, -14.99999999999999645, -10.00000000000000178 ) ) ;
#10161 = CARTESIAN_POINT ( 'NONE',  ( 47.74827507625478518, 52.59948385550239180, 7.007379884777227730 ) ) ;
#10162 = FACE_OUTER_BOUND ( 'NONE', #13127, .T. ) ;
#10163 = CARTESIAN_POINT ( 'NONE',  ( 43.34962307344078880, 46.10051614449766078, -2.184720259617096705 ) ) ;
#10164 = DIRECTION ( 'NONE',  ( 0.8090169943749464521, 0.5877852522924744694, 0.000000000000000000 ) ) ;
#10165 = FACE_BOUND ( 'NONE', #5954, .T. ) ;
#10166 = AXIS2_PLACEMENT_3D ( 'NONE', #13594, #6340, #12117 ) ;
#10167 = LINE ( 'NONE', #87, #15051 ) ;
#10168 = ADVANCED_FACE ( 'NONE', ( #7027 ), #15959, .F. ) ;
#10169 = ORIENTED_EDGE ( 'NONE', *, *, #18097, .T. ) ;
#10170 = ORIENTED_EDGE ( 'NONE', *, *, #9882, .T. ) ;
#10171 = CARTESIAN_POINT ( 'NONE',  ( -154.9999999999999716, -14.99999999999999645, 15.00000000000000000 ) ) ;
#10172 = CIRCLE ( 'NONE', #16156, 5.000000000000007994 ) ;
#10173 = DIRECTION ( 'NONE',  ( 1.000000000000000000, 0.000000000000000000, 0.000000000000000000 ) ) ;
#10174 = SURFACE_SIDE_STYLE ('',( #19134 ) ) ;
#10175 = ORIENTED_EDGE ( 'NONE', *, *, #4232, .T. ) ;
#10176 = CARTESIAN_POINT ( 'NONE',  ( 6.207530437345011087, 3.810448612249821565, 3.400109403952575882 ) ) ;
#10177 = ORIENTED_EDGE ( 'NONE', *, *, #1001, .F. ) ;
#10178 = VERTEX_POINT ( 'NONE', #7125 ) ;
#10179 = DIRECTION ( 'NONE',  ( 1.000000000000000000, -0.000000000000000000, 0.000000000000000000 ) ) ;
#10180 = CARTESIAN_POINT ( 'NONE',  ( 56.30877334542961421, 49.00051614449765935, 0.02388180880515774693 ) ) ;
#10181 = DIRECTION ( 'NONE',  ( -1.000000000000000000, 0.000000000000000000, 0.000000000000000000 ) ) ;
#10182 = CIRCLE ( 'NONE', #18976, 5.999999999999977796 ) ;
#10183 = DIRECTION ( 'NONE',  ( 1.000000000000000000, 0.000000000000000000, 0.000000000000000000 ) ) ;
#10184 = CARTESIAN_POINT ( 'NONE',  ( 46.49166364869460466, 48.69948385550241454, 4.867452303228209765 ) ) ;
#10185 = LINE ( 'NONE', #889, #14760 ) ;
#10186 = CARTESIAN_POINT ( 'NONE',  ( 55.96859303347804371, 54.19948385550240033, 4.306917132069425946 ) ) ;
#10187 = CARTESIAN_POINT ( 'NONE',  ( 49.97728705011495265, 49.50051614449766646, 8.000000000000001776 ) ) ;
#10188 = CARTESIAN_POINT ( 'NONE',  ( 0.05140428708382505096, -3.841181488860373250, 3.346878500200758833 ) ) ;
#10189=STYLED_ITEM('',(#19468),#2030);
#10190 = CARTESIAN_POINT ( 'NONE',  ( 2.449293598294706513E-15, -20.00000000000000000, -9.000000000000000000 ) ) ;
#10191 =( NAMED_UNIT ( * ) PLANE_ANGLE_UNIT ( ) SI_UNIT ( $, .RADIAN. ) );
#10192 = ORIENTED_EDGE ( 'NONE', *, *, #6163, .F. ) ;
#10193 = DIRECTION ( 'NONE',  ( 1.000000000000000000, -0.000000000000000000, -0.000000000000000000 ) ) ;
#10194 = AXIS2_PLACEMENT_3D ( 'NONE', #5580, #16275, #8617 ) ;
#10195 = DIRECTION ( 'NONE',  ( -0.000000000000000000, -0.000000000000000000, -1.000000000000000000 ) ) ;
#10196 = CYLINDRICAL_SURFACE ( 'NONE', #3743, 7.500000000000000888 ) ;
#10197 = CIRCLE ( 'NONE', #1772, 1.000000000000000444 ) ;
#10198 = CARTESIAN_POINT ( 'NONE',  ( -16.79901371501587803, -9.146745271453902149, 0.000000000000000000 ) ) ;
#10199 = CARTESIAN_POINT ( 'NONE',  ( 14.86289650954772590, -6.617387872822656725, 9.000000000000000000 ) ) ;
#10200 = PLANE ( 'NONE',  #12337 ) ;
#10201 = CARTESIAN_POINT ( 'NONE',  ( 1.274258131564866448, 3.883108878240963513, -3.220599429844046568 ) ) ;
#10202 = CARTESIAN_POINT ( 'NONE',  ( 44.03140696652192787, 55.19948385550238612, -4.306917132069425058 ) ) ;
#10203 = DIRECTION ( 'NONE',  ( 0.000000000000000000, 0.000000000000000000, -1.000000000000000000 ) ) ;
#10204 = AXIS2_PLACEMENT_3D ( 'NONE', #18479, #5215, #8157 ) ;
#10205 = CARTESIAN_POINT ( 'NONE',  ( 54.72065718078924590, 48.29948385550240175, 6.458785618021043895 ) ) ;
#10206 = EDGE_CURVE ( 'NONE', #14027, #8364, #8323, .T. ) ;
#10207 = CARTESIAN_POINT ( 'NONE',  ( 57.36023556966787851, 49.00051614449763804, 0.02388180880515038476 ) ) ;
#10208 = CARTESIAN_POINT ( 'NONE',  ( 9.999999999999994671, 20.00000000000001421, 15.00000000000000000 ) ) ;
#10209 = PRODUCT_DEFINITION ( 'UNKNOWN', '', #14488, #13426 ) ;
#10210 = ORIENTED_EDGE ( 'NONE', *, *, #11285, .F. ) ;
#10211 = EDGE_CURVE ( 'NONE', #3558, #6641, #13103, .T. ) ;
#10212 = ORIENTED_EDGE ( 'NONE', *, *, #18036, .F. ) ;
#10213 = CARTESIAN_POINT ( 'NONE',  ( 1.000000000000000444, -15.10102051443364246, -8.999999999999998224 ) ) ;
#10214 = ORIENTED_EDGE ( 'NONE', *, *, #6869, .F. ) ;
#10215 = EDGE_CURVE ( 'NONE', #6434, #7511, #16308, .T. ) ;
#10216 = EDGE_CURVE ( 'NONE', #19213, #7928, #4187, .T. ) ;
#10217 = CIRCLE ( 'NONE', #15876, 0.7500000000000002220 ) ;
#10218 = DIRECTION ( 'NONE',  ( 1.000000000000000000, 0.000000000000000000, 0.000000000000000000 ) ) ;
#10219 = VECTOR ( 'NONE', #9673, 1000.000000000000000 ) ;
#10220 = ORIENTED_EDGE ( 'NONE', *, *, #13706, .T. ) ;
#10221 = CYLINDRICAL_SURFACE ( 'NONE', #19152, 4.000000000000003553 ) ;
#10222 = EDGE_CURVE ( 'NONE', #1748, #12905, #5653, .T. ) ;
#10223 = EDGE_LOOP ( 'NONE', ( #2547, #7713, #3084, #14366 ) ) ;
#10224 = CARTESIAN_POINT ( 'NONE',  ( 2.449293598294706513E-15, -20.00000000000000000, -9.999999999999994671 ) ) ;
#10225 = ORIENTED_EDGE ( 'NONE', *, *, #11908, .T. ) ;
#10226 = CARTESIAN_POINT ( 'NONE',  ( 43.20883090819745576, 56.79948385550240175, 4.963592699179006473 ) ) ;
#10227 = DIRECTION ( 'NONE',  ( 1.000000000000000000, 0.000000000000000000, 0.000000000000000000 ) ) ;
#10228 = AXIS2_PLACEMENT_3D ( 'NONE', #17078, #16786, #3449 ) ;
#10229 = PRODUCT_DEFINITION_SHAPE ( 'NONE', 'NONE',  #19425 ) ;
#10230 = CARTESIAN_POINT ( 'NONE',  ( 44.91013252490152752, 54.79948385550240175, 3.727524721679198461 ) ) ;
#10231 = CARTESIAN_POINT ( 'NONE',  ( 6.196878017913830305, -3.367876570272811509, 4.166666666666666963 ) ) ;
#10232 = DIRECTION ( 'NONE',  ( -0.000000000000000000, -0.000000000000000000, -1.000000000000000000 ) ) ;
#10233 = CARTESIAN_POINT ( 'NONE',  ( 54.72065718078918906, 46.70051614449766220, -6.458785618021089192 ) ) ;
#10234 = EDGE_CURVE ( 'NONE', #12595, #15728, #627, .T. ) ;
#10235 = CARTESIAN_POINT ( 'NONE',  ( 55.69932041026405045, 51.10051614449766078, 1.875703265242156359 ) ) ;
#10236 = EDGE_CURVE ( 'NONE', #17826, #11915, #17922, .T. ) ;
#10237 = CARTESIAN_POINT ( 'NONE',  ( -154.9999999999999716, -14.99999999999999645, 3.999999999999999112 ) ) ;
#10238=STYLED_ITEM('',(#19475),#8395);
#10239 = FACE_OUTER_BOUND ( 'NONE', #13398, .T. ) ;
#10240 = ORIENTED_EDGE ( 'NONE', *, *, #10206, .F. ) ;
#10241 = ORIENTED_EDGE ( 'NONE', *, *, #2274, .T. ) ;
#10242 = DIRECTION ( 'NONE',  ( -1.000000000000000000, -0.000000000000000000, -0.000000000000000000 ) ) ;
#10243 = VERTEX_POINT ( 'NONE', #16541 ) ;
#10244 = CARTESIAN_POINT ( 'NONE',  ( 44.05948171654949874, 64.79948385550240175, 4.345558710429105354 ) ) ;
#10245 = CIRCLE ( 'NONE', #544, 0.4999999999999972244 ) ;
#10246 = ORIENTED_EDGE ( 'NONE', *, *, #2723, .F. ) ;
#10247 = ORIENTED_EDGE ( 'NONE', *, *, #2519, .T. ) ;
#10248 = DIRECTION ( 'NONE',  ( 1.000000000000000000, 0.000000000000000000, 0.000000000000000000 ) ) ;
#10249 = DIRECTION ( 'NONE',  ( -1.000000000000000000, -0.000000000000000000, -0.000000000000000000 ) ) ;
#10250 = CONICAL_SURFACE ( 'NONE', #1814, 5.000000000000000000, 1.047197551196600296 ) ;
#10251 = ORIENTED_EDGE ( 'NONE', *, *, #8915, .F. ) ;
#10252 = CARTESIAN_POINT ( 'NONE',  ( -1.250000000000001110, 0.000000000000000000, 0.000000000000000000 ) ) ;
#10253 = ORIENTED_EDGE ( 'NONE', *, *, #15623, .F. ) ;
#10254 = CONICAL_SURFACE ( 'NONE', #11809, 1.999999999999998224, 1.029744259999999745 ) ;
#10255 = CARTESIAN_POINT ( 'NONE',  ( -3.436319922987618902, 2.634841920961291439, -3.531542292955721862 ) ) ;
#10256 = CARTESIAN_POINT ( 'NONE',  ( 47.70284917648453415, 53.39948385550238186, -6.992620115222774047 ) ) ;
#10257 = FACE_OUTER_BOUND ( 'NONE', #2458, .T. ) ;
#10258 = CARTESIAN_POINT ( 'NONE',  ( 57.36023556966787851, 49.00051614449763804, 0.02388180880515038476 ) ) ;
#10259 = FACE_OUTER_BOUND ( 'NONE', #5225, .T. ) ;
#10260 = SURFACE_STYLE_FILL_AREA ( #4499 ) ;
#10261 = DIRECTION ( 'NONE',  ( 1.000000000000000000, 0.000000000000000000, -0.000000000000000000 ) ) ;
#10262 = AXIS2_PLACEMENT_3D ( 'NONE', #11005, #15330, #2299 ) ;
#10263 = AXIS2_PLACEMENT_3D ( 'NONE', #19253, #16395, #16295 ) ;
#10264 = ORIENTED_EDGE ( 'NONE', *, *, #4249, .F. ) ;
#10265 = VERTEX_POINT ( 'NONE', #11819 ) ;
#10266 = CARTESIAN_POINT ( 'NONE',  ( -7.499999999999998224, -20.00000000000000000, -10.00000000000000000 ) ) ;
#10267 =( NAMED_UNIT ( * ) SI_UNIT ( $, .STERADIAN. ) SOLID_ANGLE_UNIT ( ) );
#10268 = CARTESIAN_POINT ( 'NONE',  ( 50.02271294988512551, 48.49948385550240459, 7.000000000000000888 ) ) ;
#10269 = CARTESIAN_POINT ( 'NONE',  ( 1.925929944387235853E-31, 15.00000000000001599, -9.000000000000001776 ) ) ;
#10270 = PRESENTATION_LAYER_ASSIGNMENT (  '', '', ( #15290 ) ) ;
#10271 = ORIENTED_EDGE ( 'NONE', *, *, #4838, .F. ) ;
#10272 = LINE ( 'NONE', #6954, #1766 ) ;
#10273 = ORIENTED_EDGE ( 'NONE', *, *, #11670, .F. ) ;
#10274 = EDGE_LOOP ( 'NONE', ( #12319, #9947, #18599 ) ) ;
#10275 = AXIS2_PLACEMENT_3D ( 'NONE', #8413, #7147, #14393 ) ;
#10276 = EDGE_CURVE ( 'NONE', #4901, #18786, #17248, .T. ) ;
#10277 = AXIS2_PLACEMENT_3D ( 'NONE', #1774, #11060, #2060 ) ;
#10278 = DIRECTION ( 'NONE',  ( -0.000000000000000000, 1.000000000000000000, -0.000000000000000000 ) ) ;
#10279 = UNCERTAINTY_MEASURE_WITH_UNIT (LENGTH_MEASURE( 1.000000000000000082E-05 ), #17868, 'distance_accuracy_value', 'NONE');
#10280 = DIRECTION ( 'NONE',  ( 1.000000000000000000, 0.000000000000000000, 0.000000000000000000 ) ) ;
#10281 =( REPRESENTATION_RELATIONSHIP ('NONE','NONE', #16703, #11935 ) REPRESENTATION_RELATIONSHIP_WITH_TRANSFORMATION ( #18448 )SHAPE_REPRESENTATION_RELATIONSHIP( ) );
#10282 = CARTESIAN_POINT ( 'NONE',  ( 55.08986747509849380, 49.20051614449766220, 3.727524721679155384 ) ) ;
#10283 = CARTESIAN_POINT ( 'NONE',  ( 18.00000000000000355, -20.00000000000000000, -20.00000000000000000 ) ) ;
#10284 = ADVANCED_FACE ( 'NONE', ( #6049 ), #10648, .T. ) ;
#10285 = CARTESIAN_POINT ( 'NONE',  ( 5.000000000000003553, -20.00000000000000000, 15.00000000000000355 ) ) ;
#10286 = CARTESIAN_POINT ( 'NONE',  ( 51.97223112728254790, 60.39948385550241028, 5.992620115222778487 ) ) ;
#10287 = DIRECTION ( 'NONE',  ( -1.000000000000000000, -0.000000000000000000, -0.000000000000000000 ) ) ;
#10288 = CARTESIAN_POINT ( 'NONE',  ( 56.66441430157296821, 50.09948385550240602, 2.141517661632100111 ) ) ;
#10289 = CARTESIAN_POINT ( 'NONE',  ( 43.20883090819742023, 50.20051614449766220, -4.963592699178938972 ) ) ;
#10290 = CARTESIAN_POINT ( 'NONE',  ( 4.071447262713888016, -2.020725942163694722, -3.499999999999999556 ) ) ;
#10291 = DIRECTION ( 'NONE',  ( 0.000000000000000000, 0.000000000000000000, -1.000000000000000000 ) ) ;
#10292 = AXIS2_PLACEMENT_3D ( 'NONE', #13388, #1438, #7413 ) ;
#10293 = AXIS2_PLACEMENT_3D ( 'NONE', #13972, #15457, #13880 ) ;
#10294 = DIRECTION ( 'NONE',  ( 0.8513098556990980059, 0.5246632535156059429, 2.775557561562891351E-17 ) ) ;
#10295 = ORIENTED_EDGE ( 'NONE', *, *, #1179, .T. ) ;
#10296 = CARTESIAN_POINT ( 'NONE',  ( 2.449293598294706513E-15, -20.00000000000000000, 9.000000000000000000 ) ) ;
#10297 = CARTESIAN_POINT ( 'NONE',  ( 2.449293598294706513E-15, -20.00000000000000000, 9.000000000000000000 ) ) ;
#10298 = CYLINDRICAL_SURFACE ( 'NONE', #11248, 2.649999999999985700 ) ;
#10299 = FACE_OUTER_BOUND ( 'NONE', #2319, .T. ) ;
#10300 = DIRECTION ( 'NONE',  ( 1.000000000000000000, 0.000000000000000000, 0.000000000000000000 ) ) ;
#10301 = CIRCLE ( 'NONE', #15946, 0.2000000000000000944 ) ;
#10302 = CARTESIAN_POINT ( 'NONE',  ( 10.93224627749287592, -3.252283996668583033, 0.000000000000000000 ) ) ;
#10303 = CIRCLE ( 'NONE', #7178, 20.00000000000000000 ) ;
#10304 = DIRECTION ( 'NONE',  ( 0.02857142857142857054, -0.9995917534020515305, 0.000000000000000000 ) ) ;
#10305 = CARTESIAN_POINT ( 'NONE',  ( 44.05948171654949874, 54.79948385550241596, 4.345558710429105354 ) ) ;
#10306 = LINE ( 'NONE', #9223, #11942 ) ;
#10307 = CARTESIAN_POINT ( 'NONE',  ( 47.42335538002188144, 50.59948385550240602, 8.007379884777233059 ) ) ;
#10308 = CARTESIAN_POINT ( 'NONE',  ( 3.958484000407238579, -3.734437307742088485, -0.5317648453099828032 ) ) ;
#10309 = CARTESIAN_POINT ( 'NONE',  ( 54.09612160359792199, 47.30051614449765651, 5.676469297603124353 ) ) ;
#10310 = CIRCLE ( 'NONE', #4071, 6.080745460913608902 ) ;
#10311 = CARTESIAN_POINT ( 'NONE',  ( -54.99999999999996447, -14.99999999999998579, -10.00000000000000178 ) ) ;
#10312 = ORIENTED_EDGE ( 'NONE', *, *, #766, .T. ) ;
#10313 = ORIENTED_EDGE ( 'NONE', *, *, #10396, .F. ) ;
#10314 = CARTESIAN_POINT ( 'NONE',  ( -0.1713913650100259145, 0.000000000000000000, 0.000000000000000000 ) ) ;
#10315 = VERTEX_POINT ( 'NONE', #11916 ) ;
#10316 = CARTESIAN_POINT ( 'NONE',  ( 0.1713913650100259145, 6.016077400811372436E-16, -4.424999999999999822 ) ) ;
#10317 = ORIENTED_EDGE ( 'NONE', *, *, #2312, .T. ) ;
#10318 = DIRECTION ( 'NONE',  ( -0.7779254092217071648, -0.6283566325640553840, 0.000000000000000000 ) ) ;
#10319 = EDGE_CURVE ( 'NONE', #14876, #1343, #14959, .T. ) ;
#10320 = EDGE_LOOP ( 'NONE', ( #14154, #8103, #16321, #5623 ) ) ;
#10321 = AXIS2_PLACEMENT_3D ( 'NONE', #351, #4852, #6500 ) ;
#10322 = DIRECTION ( 'NONE',  ( 0.04542589977017006536, -0.9989677110047503472, 0.000000000000000000 ) ) ;
#10323 = ORIENTED_EDGE ( 'NONE', *, *, #3817, .T. ) ;
#10324 = DIRECTION ( 'NONE',  ( -0.000000000000000000, -0.000000000000000000, 1.000000000000000000 ) ) ;
#10325 = DIRECTION ( 'NONE',  ( 0.000000000000000000, 0.000000000000000000, 1.000000000000000000 ) ) ;
#10326 = CARTESIAN_POINT ( 'NONE',  ( 55.71335778527780747, 60.09948385550240602, 1.832500667257165983 ) ) ;
#10327 = PLANE ( 'NONE',  #1658 ) ;
#10328 = CARTESIAN_POINT ( 'NONE',  ( 2.449293598294706513E-15, -20.00000000000000000, -23.00000000000000000 ) ) ;
#10329 = CARTESIAN_POINT ( 'NONE',  ( 52.57664461997821093, 51.40051614449767214, 8.007379884777206414 ) ) ;
#10330 = AXIS2_PLACEMENT_3D ( 'NONE', #8226, #15485, #6755 ) ;
#10331 = CARTESIAN_POINT ( 'NONE',  ( 46.49166364869456913, 50.30051614449766362, -4.867452303228181343 ) ) ;
#10333 = AXIS2_PLACEMENT_3D ( 'NONE', #8607, #2452, #12925 ) ;
#10332 = CARTESIAN_POINT ( 'NONE',  ( 4.050823680195224874, -2.400527758044906701, -2.978030508226146900 ) ) ;
#10334 = AXIS2_PLACEMENT_3D ( 'NONE', #17117, #11110, #12591 ) ;
#10335 = DIRECTION ( 'NONE',  ( -0.000000000000000000, 0.000000000000000000, 1.000000000000000000 ) ) ;
#10336 = ORIENTED_EDGE ( 'NONE', *, *, #12551, .F. ) ;
#10337 = ADVANCED_FACE ( 'NONE', ( #8975 ), #3212, .F. ) ;
#10338 = AXIS2_PLACEMENT_3D ( 'NONE', #11879, #7382, #17887 ) ;
#10339 = ORIENTED_EDGE ( 'NONE', *, *, #2087, .F. ) ;
#10340 = DIRECTION ( 'NONE',  ( 0.000000000000000000, 0.000000000000000000, -1.000000000000000000 ) ) ;
#10341 = ORIENTED_EDGE ( 'NONE', *, *, #184, .F. ) ;
#10342 = CARTESIAN_POINT ( 'NONE',  ( -3.574908632038010113E-15, 4.821944789745366222, -1.648146632869000427 ) ) ;
#10343 = PLANE ( 'NONE',  #4692 ) ;
#10344 = ORIENTED_EDGE ( 'NONE', *, *, #5737, .F. ) ;
#10345 = DIRECTION ( 'NONE',  ( 1.000000000000000000, 0.000000000000000000, 0.000000000000000000 ) ) ;
#10346 = VECTOR ( 'NONE', #16179, 1000.000000000000000 ) ;
#10347 = EDGE_CURVE ( 'NONE', #1565, #18734, #7607, .T. ) ;
#10348 = CARTESIAN_POINT ( 'NONE',  ( 47.74827507625477807, 48.59948385550239891, 7.007379884777229506 ) ) ;
#10349 = EDGE_CURVE ( 'NONE', #16533, #3206, #2211, .T. ) ;
#10350 = EDGE_LOOP ( 'NONE', ( #5178, #19382, #8755, #2022 ) ) ;
#10351 = VECTOR ( 'NONE', #18421, 1000.000000000000000 ) ;
#10352 = CARTESIAN_POINT ( 'NONE',  ( 4.175813232069148562, 4.122719923832741884, -2.765695189283172261E-17 ) ) ;
#10353 = AXIS2_PLACEMENT_3D ( 'NONE', #9741, #16033, #2617 ) ;
#10354 = ORIENTED_EDGE ( 'NONE', *, *, #9791, .T. ) ;
#10355 = AXIS2_PLACEMENT_3D ( 'NONE', #3004, #16338, #7309 ) ;
#10356 = CARTESIAN_POINT ( 'NONE',  ( 2.449293598294706513E-15, -20.00000000000000000, 9.000000000000000000 ) ) ;
#10357 = CARTESIAN_POINT ( 'NONE',  ( 43.33558569842703179, 55.09948385550241312, -2.141517661632099223 ) ) ;
#10358 = DIRECTION ( 'NONE',  ( 1.000000000000000000, 0.000000000000000000, 0.000000000000000000 ) ) ;
#10359 = AXIS2_PLACEMENT_3D ( 'NONE', #2871, #8834, #16191 ) ;
#10360 = CARTESIAN_POINT ( 'NONE',  ( 47.70284917648459100, 55.60051614449764656, 6.992620115222796251 ) ) ;
#10361 = CARTESIAN_POINT ( 'NONE',  ( -159.0000000000000000, -14.99999999999999645, 17.00000000000000000 ) ) ;
#10362 = EDGE_CURVE ( 'NONE', #11836, #18140, #5850, .T. ) ;
#10363 =( NAMED_UNIT ( * ) PLANE_ANGLE_UNIT ( ) SI_UNIT ( $, .RADIAN. ) );
#10364 = ADVANCED_FACE ( 'NONE', ( #3115 ), #2824, .T. ) ;
#10365 = CARTESIAN_POINT ( 'NONE',  ( -4.203934362469166963, -1.640673743454851286, -3.598432614606932756 ) ) ;
#10366 = ORIENTED_EDGE ( 'NONE', *, *, #9176, .F. ) ;
#10367 = ADVANCED_FACE ( 'NONE', ( #13294 ), #4678, .F. ) ;
#10368 = CIRCLE ( 'NONE', #19167, 4.100000000000000533 ) ;
#10369 = ORIENTED_EDGE ( 'NONE', *, *, #635, .T. ) ;
#10370 = ORIENTED_EDGE ( 'NONE', *, *, #1846, .T. ) ;
#10371 = CARTESIAN_POINT ( 'NONE',  ( 0.3126073911696407026, -2.020725942163686728, 3.500000000000000444 ) ) ;
#10372 = CIRCLE ( 'NONE', #10060, 4.872650870659752442 ) ;
#10373 = CARTESIAN_POINT ( 'NONE',  ( 44.05948171654949874, 48.79948385550238754, 4.345558710429105354 ) ) ;
#10374 = CARTESIAN_POINT ( 'NONE',  ( 20.00000000000000000, -25.00000000000000711, -23.00000000000000000 ) ) ;
#10375 = EDGE_LOOP ( 'NONE', ( #12524, #14757, #2290, #10434 ) ) ;
#10376 = LINE ( 'NONE', #8102, #16479 ) ;
#10377 = ORIENTED_EDGE ( 'NONE', *, *, #16491, .T. ) ;
#10378 = CARTESIAN_POINT ( 'NONE',  ( 45.90387839640208512, 56.30051614449765651, -5.676469297603124353 ) ) ;
#10379 = VERTEX_POINT ( 'NONE', #9174 ) ;
#10380 = CARTESIAN_POINT ( 'NONE',  ( 1.734723475976807094E-15, 4.618802153517012954, -0.4999999999999995559 ) ) ;
#10381 = LINE ( 'NONE', #14892, #15881 ) ;
#10382 = CARTESIAN_POINT ( 'NONE',  ( 46.45491332379576477, 49.70051614449766220, 4.840751629271188961 ) ) ;
#10383 = CARTESIAN_POINT ( 'NONE',  ( 19.02113032590300890, -13.81966011250085025, -9.000000000000000000 ) ) ;
#10384 = PRODUCT_DEFINITION_SHAPE ( 'NONE', 'NONE',  #10209 ) ;
#10385 = CARTESIAN_POINT ( 'NONE',  ( 3.309651814758564736, -5.455921364805393026, -1.000000000000000000 ) ) ;
#10386 = AXIS2_PLACEMENT_3D ( 'NONE', #10745, #16746, #1837 ) ;
#10387 = CARTESIAN_POINT ( 'NONE',  ( 48.07319477248768180, 54.59948385550240602, 6.007379884777225953 ) ) ;
#10388 = FACE_OUTER_BOUND ( 'NONE', #1687, .T. ) ;
#10389 = CARTESIAN_POINT ( 'NONE',  ( 56.65037692655918988, 53.89948385550240317, -2.184720259617163762 ) ) ;
#10390 = CARTESIAN_POINT ( 'NONE',  ( 56.79116909180259398, 55.20051614449766220, 4.963592699178938972 ) ) ;
#10391 = B_SPLINE_CURVE_WITH_KNOTS ( 'NONE', 3,
 ( #9329, #12179, #15413, #15221, #18377, #16706 ),
 .UNSPECIFIED., .F., .F.,
 ( 4, 2, 4 ),
 ( 0.01308430720669670130, 0.01410661709916351952, 0.01512892699163033601 ),
 .UNSPECIFIED. ) ;
#10392 = CARTESIAN_POINT ( 'NONE',  ( -4.000000000000000000, 2.309401076758498483, -0.4999999999999927280 ) ) ;
#10393 = CARTESIAN_POINT ( 'NONE',  ( -4.197393957002303999, -7.773935952363655451E-14, -3.503767560748929810 ) ) ;
#10394 = ORIENTED_EDGE ( 'NONE', *, *, #8931, .T. ) ;
#10395 = CARTESIAN_POINT ( 'NONE',  ( -74.99999999999997158, -40.00000000000000000, -10.00000000000000000 ) ) ;
#10396 = EDGE_CURVE ( 'NONE', #3609, #7688, #14719, .T. ) ;
#10397 = B_SPLINE_CURVE_WITH_KNOTS ( 'NONE', 3,
 ( #13504, #10448, #17932, #3020, #18023, #12310, #4584, #6056, #2925, #9263, #16549, #4490 ),
 .UNSPECIFIED., .F., .F.,
 ( 4, 2, 2, 2, 2, 4 ),
 ( 0.01755862241325779893, 0.01812962329865995884, 0.01870062418406211874, 0.01984262595486643854, 0.02098462772567075835, 0.02212662949647507815 ),
 .UNSPECIFIED. ) ;
#10398 = ORIENTED_EDGE ( 'NONE', *, *, #4485, .F. ) ;
#10399 = CARTESIAN_POINT ( 'NONE',  ( -1.000000000000000222, -4.808326913195983821, -0.8000000000000000444 ) ) ;
#10400 = ADVANCED_FACE ( 'NONE', ( #18017 ), #4577, .T. ) ;
#10401 = PLANE ( 'NONE',  #4703 ) ;
#10402 = DIRECTION ( 'NONE',  ( 1.000000000000000000, 0.000000000000000000, 0.000000000000000000 ) ) ;
#10403 = DIRECTION ( 'NONE',  ( 1.000000000000000000, 0.000000000000000000, 0.000000000000000000 ) ) ;
#10404 = CYLINDRICAL_SURFACE ( 'NONE', #19261, 1.000000000000000888 ) ;
#10405 = CARTESIAN_POINT ( 'NONE',  ( 73.00000000000000000, 3.000000000000000000, -5.999999999999998224 ) ) ;
#10406 = CARTESIAN_POINT ( 'NONE',  ( 54.13287192849676188, 56.29948385550240175, 5.649768623646098220 ) ) ;
#10407 = VECTOR ( 'NONE', #16935, 1000.000000000000000 ) ;
#10408 = CYLINDRICAL_SURFACE ( 'NONE', #6619, 2.500000000000000444 ) ;
#10409 = CARTESIAN_POINT ( 'NONE',  ( 52.62207051974839089, 52.39948385550241028, 7.992620115222770494 ) ) ;
#10410 = FACE_OUTER_BOUND ( 'NONE', #14046, .T. ) ;
#10411 = CARTESIAN_POINT ( 'NONE',  ( 45.90387839640208512, 52.30051614449766362, -5.676469297603124353 ) ) ;
#10412 = ADVANCED_FACE ( 'NONE', ( #8145 ), #9409, .F. ) ;
#10413 = DIRECTION ( 'NONE',  ( 1.000000000000000000, 0.000000000000000000, 0.000000000000000000 ) ) ;
#10414 = ORIENTED_EDGE ( 'NONE', *, *, #8782, .F. ) ;
#10415 = EDGE_LOOP ( 'NONE', ( #10418, #4357, #14372, #9306 ) ) ;
#10416 = VERTEX_POINT ( 'NONE', #12206 ) ;
#10417 = CARTESIAN_POINT ( 'NONE',  ( -164.9999999999999716, -14.99999999999999645, -4.000000000000000000 ) ) ;
#10418 = ORIENTED_EDGE ( 'NONE', *, *, #10579, .F. ) ;
#10419 = CARTESIAN_POINT ( 'NONE',  ( 4.200000000000001954, 0.000000000000000000, -2.200000000000001066 ) ) ;
#10420 = EDGE_LOOP ( 'NONE', ( #17696, #9772, #15926, #15665 ) ) ;
#10421 = CARTESIAN_POINT ( 'NONE',  ( 2.449293598294706513E-15, -20.00000000000000000, -8.999999999999998224 ) ) ;
#10422 = PRODUCT_DEFINITION_FORMATION_WITH_SPECIFIED_SOURCE ( 'ANY', '', #6944, .NOT_KNOWN. ) ;
#10423 = VERTEX_POINT ( 'NONE', #8786 ) ;
#10424 = CARTESIAN_POINT ( 'NONE',  ( 4.630153689607048761, 0.000000000000000000, -5.371010071662833063 ) ) ;
#10425 = CARTESIAN_POINT ( 'NONE',  ( -16.32050807568872841, -30.00000000000008171, -9.000000000000000000 ) ) ;
#10426 = CARTESIAN_POINT ( 'NONE',  ( 55.08986747509847248, 55.79948385550239465, -3.727524721679197572 ) ) ;
#10427 = CARTESIAN_POINT ( 'NONE',  ( -3.309651814758565180, -5.455921364805393026, -1.000000000000000000 ) ) ;
#10428 = CARTESIAN_POINT ( 'NONE',  ( -154.9999999999999716, -14.99999999999999645, 15.00000000000000000 ) ) ;
#10429 = CARTESIAN_POINT ( 'NONE',  ( 54.68390685589039890, 55.30051614449765651, 6.485486291978072693 ) ) ;
#10430 = CARTESIAN_POINT ( 'NONE',  ( 44.28664221472221385, 47.90051614449765793, 1.832500667257213722 ) ) ;
#10431 = DIRECTION ( 'NONE',  ( -0.9999670257950099561, -0.008120795692649453515, 0.000000000000000000 ) ) ;
#10432 = DIRECTION ( 'NONE',  ( 0.000000000000000000, 0.000000000000000000, -1.000000000000000000 ) ) ;
#10433 = ORIENTED_EDGE ( 'NONE', *, *, #2710, .T. ) ;
#10434 = ORIENTED_EDGE ( 'NONE', *, *, #3888, .T. ) ;
#10435 = CARTESIAN_POINT ( 'NONE',  ( -32.00000000000000000, 3.000000000000000000, 6.000000000000000000 ) ) ;
#10436 = EDGE_LOOP ( 'NONE', ( #16127, #15628, #1999 ) ) ;
#10437 = CARTESIAN_POINT ( 'NONE',  ( 56.65037692655918988, 61.89948385550241028, -2.184720259617163762 ) ) ;
#10438 = DIRECTION ( 'NONE',  ( -0.000000000000000000, 0.000000000000000000, 1.000000000000000000 ) ) ;
#10439 = ORIENTED_EDGE ( 'NONE', *, *, #5807, .T. ) ;
#10440 = DIRECTION ( 'NONE',  ( -1.000000000000000000, -0.000000000000000000, -0.000000000000000000 ) ) ;
#10441 = CARTESIAN_POINT ( 'NONE',  ( 54.09612160359786515, 45.69948385550240744, -5.676469297603166098 ) ) ;
#10442 = AXIS2_PLACEMENT_3D ( 'NONE', #11996, #49, #13660 ) ;
#10443 = ORIENTED_EDGE ( 'NONE', *, *, #6050, .T. ) ;
#10444 = DIRECTION ( 'NONE',  ( 0.000000000000000000, 0.000000000000000000, 1.000000000000000000 ) ) ;
#10445 = ORIENTED_EDGE ( 'NONE', *, *, #3526, .F. ) ;
#10446 = CARTESIAN_POINT ( 'NONE',  ( 43.18075615816989199, 47.19948385550240744, -4.924951120819313743 ) ) ;
#10447 = VECTOR ( 'NONE', #13509, 1000.000000000000000 ) ;
#10448 = CARTESIAN_POINT ( 'NONE',  ( 54.08601618280673051, 45.00000000000005684, -5.120135501906166731 ) ) ;
#10449 = CARTESIAN_POINT ( 'NONE',  ( 47.74827507625478518, 60.59948385550239891, 7.007379884777227730 ) ) ;
#10450 = CARTESIAN_POINT ( 'NONE',  ( -10.75570504584937304, -36.18033988749900942, 9.000000000000000000 ) ) ;
#10451 = CARTESIAN_POINT ( 'NONE',  ( 45.90387839640208512, 52.30051614449766362, -5.676469297603124353 ) ) ;
#10452 = FACE_OUTER_BOUND ( 'NONE', #11212, .T. ) ;
#10453 = FILL_AREA_STYLE ('',( #9793 ) ) ;
#10454 = CYLINDRICAL_SURFACE ( 'NONE', #18207, 7.500000000000000888 ) ;
#10455 = ORIENTED_EDGE ( 'NONE', *, *, #1670, .T. ) ;
#10456 = EDGE_CURVE ( 'NONE', #9345, #19206, #26, .T. ) ;
#10457 = ORIENTED_EDGE ( 'NONE', *, *, #9373, .T. ) ;
#10458 = ORIENTED_EDGE ( 'NONE', *, *, #18185, .F. ) ;
#10459 = PLANE ( 'NONE',  #19394 ) ;
#10460 = PRESENTATION_STYLE_ASSIGNMENT (( #182 ) ) ;
#10461 = AXIS2_PLACEMENT_3D ( 'NONE', #8623, #3732, #8231 ) ;
#10462 = EDGE_CURVE ( 'NONE', #7491, #18559, #15357, .T. ) ;
#10463 = CARTESIAN_POINT ( 'NONE',  ( 49.97728705011488159, 47.49948385550240459, -7.000000000000000888 ) ) ;
#10464 = VERTEX_POINT ( 'NONE', #7695 ) ;
#10465 = DIRECTION ( 'NONE',  ( 0.000000000000000000, 1.000000000000000000, -1.224646799147353207E-16 ) ) ;
#10466 = EDGE_CURVE ( 'NONE', #8974, #17434, #16938, .T. ) ;
#10467 = EDGE_CURVE ( 'NONE', #1806, #12622, #4282, .T. ) ;
#10468 = VERTEX_POINT ( 'NONE', #15536 ) ;
#10469 = CARTESIAN_POINT ( 'NONE',  ( 47.70284917648459810, 57.60051614449765367, 6.992620115222797139 ) ) ;
#10470 = ORIENTED_EDGE ( 'NONE', *, *, #1970, .F. ) ;
#10471 = EDGE_CURVE ( 'NONE', #10265, #7928, #6573, .T. ) ;
#10472 = CARTESIAN_POINT ( 'NONE',  ( 4.000000000000000000, 2.309401076758497151, -5.000000000000000000 ) ) ;
#10473 = PRODUCT_DEFINITION_CONTEXT ( 'detailed design', #14660, 'design' ) ;
#10474 = DIRECTION ( 'NONE',  ( 1.000000000000000000, 0.000000000000000000, 0.000000000000000000 ) ) ;
#10475 = AXIS2_PLACEMENT_3D ( 'NONE', #4124, #10093, #2671 ) ;
#10476 = CARTESIAN_POINT ( 'NONE',  ( 55.11794222512599362, 54.80051614449764941, -3.688883143319583446 ) ) ;
#10477 = CARTESIAN_POINT ( 'NONE',  ( -150.9999999999999432, -14.99999999999999645, -17.00000000000000000 ) ) ;
#10478 = CARTESIAN_POINT ( 'NONE',  ( 0.000000000000000000, 0.000000000000000000, -0.8000000000000000444 ) ) ;
#10479 = CARTESIAN_POINT ( 'NONE',  ( 44.88205777487398507, 57.19948385550241454, -3.688883143319540814 ) ) ;
#10480 = CARTESIAN_POINT ( 'NONE',  ( 0.5276280594147412240, -4.314175951381924889, -3.320322319201654881 ) ) ;
#10481 = EDGE_CURVE ( 'NONE', #7648, #3535, #10012, .T. ) ;
#10482 = CARTESIAN_POINT ( 'NONE',  ( 56.79116909180259398, 51.20051614449766220, 4.963592699178938972 ) ) ;
#10483 = CARTESIAN_POINT ( 'NONE',  ( 6.207671477327291853, -3.321994320370684317, 4.246137054662720622 ) ) ;
#10484 = DIRECTION ( 'NONE',  ( -0.000000000000000000, -0.000000000000000000, 1.000000000000000000 ) ) ;
#10485 = EDGE_CURVE ( 'NONE', #14568, #6799, #7535, .T. ) ;
#10486 = ORIENTED_EDGE ( 'NONE', *, *, #1871, .T. ) ;
#10487 = FACE_OUTER_BOUND ( 'NONE', #6409, .T. ) ;
#10488 = APPLICATION_PROTOCOL_DEFINITION ( 'draft international standard', 'automotive_design', 1998, #12034 ) ;
#10489 = AXIS2_PLACEMENT_3D ( 'NONE', #262, #4494, #14968 ) ;
#10490 = ORIENTED_EDGE ( 'NONE', *, *, #12984, .F. ) ;
#10491 = DIRECTION ( 'NONE',  ( 1.000000000000000000, 0.000000000000000000, 0.000000000000000000 ) ) ;
#10492 = CYLINDRICAL_SURFACE ( 'NONE', #16302, 4.799999999999999822 ) ;
#10493 = VECTOR ( 'NONE', #17269, 1000.000000000000000 ) ;
#10494 = CARTESIAN_POINT ( 'NONE',  ( 56.66441430157296821, 64.09948385550239891, 2.141517661632100111 ) ) ;
#10495 = CARTESIAN_POINT ( 'NONE',  ( 6.452281807715809059, 2.898928808472990060, 5.021091983800332947 ) ) ;
#10496 = FACE_OUTER_BOUND ( 'NONE', #11593, .T. ) ;
#10497 = DIRECTION ( 'NONE',  ( 0.000000000000000000, 0.000000000000000000, 1.000000000000000000 ) ) ;
#10498 = CARTESIAN_POINT ( 'NONE',  ( 57.36023556966787851, 57.99948385550239038, -0.02388180880522424582 ) ) ;
#10499 = CARTESIAN_POINT ( 'NONE',  ( -4.211140560182196957, 2.431303136016537803, -3.745885042887433514 ) ) ;
#10500 = CARTESIAN_POINT ( 'NONE',  ( 52.62207051974839089, 50.39948385550241738, 7.992620115222770494 ) ) ;
#10501 = CARTESIAN_POINT ( 'NONE',  ( -22.00000000000000000, -19.99999999999999289, -12.00000000000000000 ) ) ;
#10502 = CARTESIAN_POINT ( 'NONE',  ( 43.33558569842706021, 55.90051614449765793, 2.141517661632167169 ) ) ;
#10503 = ADVANCED_FACE ( 'NONE', ( #6510 ), #15993, .T. ) ;
#10504 = CARTESIAN_POINT ( 'NONE',  ( -12.54977455159124133, -4.427487078052150693, 9.000000000000000000 ) ) ;
#10505 = AXIS2_PLACEMENT_3D ( 'NONE', #6849, #1174, #11452 ) ;
#10506 = ORIENTED_EDGE ( 'NONE', *, *, #10704, .F. ) ;
#10507 = ADVANCED_FACE ( 'NONE', ( #634 ), #8176, .T. ) ;
#10508 = EDGE_LOOP ( 'NONE', ( #14928, #1773, #14563, #11159 ) ) ;
#10509 = AXIS2_PLACEMENT_3D ( 'NONE', #10961, #7738, #9486 ) ;
#10510 = CARTESIAN_POINT ( 'NONE',  ( 0.1999999999999987899, 0.000000000000000000, 0.000000000000000000 ) ) ;
#10511 = VERTEX_POINT ( 'NONE', #9543 ) ;
#10512 = CARTESIAN_POINT ( 'NONE',  ( -62.49999999999997158, 20.00000000000001421, -9.999999999999998224 ) ) ;
#10513 = CARTESIAN_POINT ( 'NONE',  ( 42.63976443033212860, 62.99948385550241170, 0.02388180880522514787 ) ) ;
#10514 = ORIENTED_EDGE ( 'NONE', *, *, #10145, .T. ) ;
#10515 = CARTESIAN_POINT ( 'NONE',  ( 1.000000000000002442, -20.00000000000000000, 8.999999999999998224 ) ) ;
#10516 = VERTEX_POINT ( 'NONE', #16926 ) ;
#10517 = DIRECTION ( 'NONE',  ( -1.000000000000000000, 0.000000000000000000, 0.000000000000000000 ) ) ;
#10518 = FACE_BOUND ( 'NONE', #2043, .T. ) ;
#10519 = EDGE_CURVE ( 'NONE', #514, #12240, #6611, .T. ) ;
#10520 = CARTESIAN_POINT ( 'NONE',  ( 49.97728705011488870, 55.49948385550241170, -6.000000000000000888 ) ) ;
#10521 = CARTESIAN_POINT ( 'NONE',  ( -4.158233816355060064, -39.56295201467614220, 9.000000000000000000 ) ) ;
#10522 = DIRECTION ( 'NONE',  ( -0.000000000000000000, 0.000000000000000000, -1.000000000000000000 ) ) ;
#10523 = CARTESIAN_POINT ( 'NONE',  ( 52.62207051974829852, 56.60051614449765367, -7.992620115222797139 ) ) ;
#10524 = EDGE_CURVE ( 'NONE', #5734, #5878, #1583, .T. ) ;
#10525 = CARTESIAN_POINT ( 'NONE',  ( 55.69932041026405045, 53.10051614449767499, 1.875703265242156359 ) ) ;
#10526 = DIRECTION ( 'NONE',  ( 0.000000000000000000, 0.000000000000000000, -1.000000000000000000 ) ) ;
#10527 = ORIENTED_EDGE ( 'NONE', *, *, #17561, .T. ) ;
#10528 = VERTEX_POINT ( 'NONE', #1825 ) ;
#10529 = LINE ( 'NONE', #13859, #601 ) ;
#10530 = VERTEX_POINT ( 'NONE', #3580 ) ;
#10531 = LINE ( 'NONE', #14858, #12990 ) ;
#10532 = CARTESIAN_POINT ( 'NONE',  ( 14.17539641854930998, -34.10879641843979471, 0.000000000000000000 ) ) ;
#10533 = ORIENTED_EDGE ( 'NONE', *, *, #19242, .F. ) ;
#10534 = DIRECTION ( 'NONE',  ( 0.000000000000000000, 0.000000000000000000, -1.000000000000000000 ) ) ;
#10535 = CARTESIAN_POINT ( 'NONE',  ( 42.63976443033212149, 48.99948385550241170, 0.02388180880522514787 ) ) ;
#10536 = CLOSED_SHELL ( 'NONE', ( #13973, #2570, #1494, #16097, #5871, #14679, #789, #14706, #3335, #1757, #10832, #2215, #6863, #8113, #12382, #7106, #2594, #2241, #6561, #12360, #3174, #6392, #18173, #1746, #5914, #2655, #13926 ) ) ;
#10537 = ORIENTED_EDGE ( 'NONE', *, *, #5478, .T. ) ;
#10538 = PLANE ( 'NONE',  #11937 ) ;
#10539 = ORIENTED_EDGE ( 'NONE', *, *, #16114, .T. ) ;
#10540 = CARTESIAN_POINT ( 'NONE',  ( 47.42335538002180328, 64.40051614449764372, -8.007379884777206414 ) ) ;
#10541 = DIRECTION ( 'NONE',  ( 1.000000000000000000, 0.000000000000000000, 0.000000000000000000 ) ) ;
#10542 = CIRCLE ( 'NONE', #6470, 5.000000000000000888 ) ;
#10543 = CARTESIAN_POINT ( 'NONE',  ( 44.03140696652192787, 61.19948385550239323, -4.306917132069425058 ) ) ;
#10544 = LINE ( 'NONE', #9266, #16460 ) ;
#10545 = CARTESIAN_POINT ( 'NONE',  ( 10.93224627749287592, -3.252283996668583477, 9.000000000000000000 ) ) ;
#10546 = CIRCLE ( 'NONE', #9289, 4.000000000000003553 ) ;
#10547 = CARTESIAN_POINT ( 'NONE',  ( 43.33558569842706021, 55.90051614449765793, 2.141517661632167169 ) ) ;
#10548 = CARTESIAN_POINT ( 'NONE',  ( 4.071447262713887127, 2.020725942163686284, -3.499999999999999556 ) ) ;
#10549 = DIRECTION ( 'NONE',  ( 1.000000000000000000, 0.000000000000000000, 0.000000000000000000 ) ) ;
#10550 = SHAPE_REPRESENTATION ( 'socket head cap screw_iso_ISO 4762 M4 x 10 - 10N', ( #10359 ), #4043 ) ;
#10551 = ORIENTED_EDGE ( 'NONE', *, *, #1783, .T. ) ;
#10552 = VERTEX_POINT ( 'NONE', #733 ) ;
#10553 = AXIS2_PLACEMENT_3D ( 'NONE', #412, #16889, #9417 ) ;
#10554 = ORIENTED_EDGE ( 'NONE', *, *, #13386, .F. ) ;
#10555 = LINE ( 'NONE', #17742, #881 ) ;
#10556 =( NAMED_UNIT ( * ) SI_UNIT ( $, .STERADIAN. ) SOLID_ANGLE_UNIT ( ) );
#10557 = VECTOR ( 'NONE', #7373, 1000.000000000000000 ) ;
#10558 = CARTESIAN_POINT ( 'NONE',  ( 41.58830220609386430, 62.99948385550241170, 0.02388180880523263147 ) ) ;
#10559 = PLANE ( 'NONE',  #6213 ) ;
#10560 = ORIENTED_EDGE ( 'NONE', *, *, #3546, .T. ) ;
#10561 = VECTOR ( 'NONE', #17035, 1000.000000000000000 ) ;
#10562 = CARTESIAN_POINT ( 'NONE',  ( -4.999999999999998224, -20.00000000000000000, -20.00000000000000000 ) ) ;
#10563 = ORIENTED_EDGE ( 'NONE', *, *, #5576, .T. ) ;
#10564 = CARTESIAN_POINT ( 'NONE',  ( 45.90387839640208512, 62.30051614449766362, -5.676469297603124353 ) ) ;
#10565 = ORIENTED_EDGE ( 'NONE', *, *, #17326, .T. ) ;
#10566 = EDGE_CURVE ( 'NONE', #14864, #12519, #5332, .T. ) ;
#10567 = CARTESIAN_POINT ( 'NONE',  ( 6.534838248920896930, -2.951765777552406878, 5.112608298763836601 ) ) ;
#10568 = DIRECTION ( 'NONE',  ( -0.000000000000000000, 0.000000000000000000, 1.000000000000000000 ) ) ;
#10569 = AXIS2_PLACEMENT_3D ( 'NONE', #6491, #12472, #5218 ) ;
#10570 = PRODUCT_DEFINITION ( 'UNKNOWN', '', #10422, #19144 ) ;
#10571 = CARTESIAN_POINT ( 'NONE',  ( 43.69122665457040000, 54.00051614449765935, -0.02388180880515696977 ) ) ;
#10572 = FACE_OUTER_BOUND ( 'NONE', #94, .T. ) ;
#10573 = DIRECTION ( 'NONE',  ( -0.000000000000000000, -0.000000000000000000, 1.000000000000000000 ) ) ;
#10574 = CARTESIAN_POINT ( 'NONE',  ( 51.92680522751233951, 57.59948385550240602, -6.007379884777223289 ) ) ;
#10575 = DIRECTION ( 'NONE',  ( -0.000000000000000000, 0.000000000000000000, -1.000000000000000000 ) ) ;
#10576 = CARTESIAN_POINT ( 'NONE',  ( 56.81924384183006538, 52.80051614449766362, -4.924951120819380357 ) ) ;
#10577 = EDGE_CURVE ( 'NONE', #10827, #13823, #445, .T. ) ;
#10578 = CARTESIAN_POINT ( 'NONE',  ( 16.79901371501595975, -30.85325472854598416, 0.000000000000000000 ) ) ;
#10579 = EDGE_CURVE ( 'NONE', #11530, #15909, #9397, .T. ) ;
#10580 = CARTESIAN_POINT ( 'NONE',  ( -4.197393957002303999, 0.4069871074557429025, -3.503767560748926257 ) ) ;
#10581 = ORIENTED_EDGE ( 'NONE', *, *, #14043, .F. ) ;
#10582 = CYLINDRICAL_SURFACE ( 'NONE', #4646, 20.00000000000000000 ) ;
#10583 =( LENGTH_UNIT ( ) NAMED_UNIT ( * ) SI_UNIT ( .MILLI., .METRE. ) );
#10584 = EDGE_CURVE ( 'NONE', #17741, #7129, #1900, .T. ) ;
#10585 = EDGE_CURVE ( 'NONE', #12060, #1649, #11904, .T. ) ;
#10586 = EDGE_LOOP ( 'NONE', ( #6131, #2981, #11427, #10077, #8883, #5093, #11000, #10152, #17365, #7694, #18915, #15669 ) ) ;
#10587 = LINE ( 'NONE', #13728, #18035 ) ;
#10588 = AXIS2_PLACEMENT_3D ( 'NONE', #9883, #12931, #8316 ) ;
#10589 = CIRCLE ( 'NONE', #18756, 4.599999999999999645 ) ;
#10590 = CARTESIAN_POINT ( 'NONE',  ( -3.309651814758565180, -5.455921364805393026, -1.000000000000000000 ) ) ;
#10591 = EDGE_CURVE ( 'NONE', #18302, #1080, #10966, .T. ) ;
#10592 = CARTESIAN_POINT ( 'NONE',  ( 54.13287192849676188, 64.29948385550241596, 5.649768623646098220 ) ) ;
#10593 = ADVANCED_FACE ( 'NONE', ( #9255 ), #15245, .T. ) ;
#10594 = CARTESIAN_POINT ( 'NONE',  ( 6.466260427357663154, 2.904280683598005730, 5.030361703432624232 ) ) ;
#10595 = CARTESIAN_POINT ( 'NONE',  ( 5.991014884144048480, 2.818925648462311528E-15, 4.999999999999999112 ) ) ;
#10596 = DIRECTION ( 'NONE',  ( 0.000000000000000000, 0.000000000000000000, 1.000000000000000000 ) ) ;
#10597 = CARTESIAN_POINT ( 'NONE',  ( 49.97728705011488159, 61.49948385550240459, -7.000000000000000888 ) ) ;
#10598 = B_SPLINE_CURVE_WITH_KNOTS ( 'NONE', 3,
 ( #11489, #11302, #14337, #6697 ),
 .UNSPECIFIED., .F., .F.,
 ( 4, 4 ),
 ( 0.002080789711329296236, 0.004173039763574516031 ),
 .UNSPECIFIED. ) ;
#10599 = FACE_OUTER_BOUND ( 'NONE', #6732, .T. ) ;
#10600 = CARTESIAN_POINT ( 'NONE',  ( 43.18075615816989199, 51.19948385550240744, -4.924951120819313743 ) ) ;
#10601 = FACE_OUTER_BOUND ( 'NONE', #11208, .T. ) ;
#10602 = PRESENTATION_LAYER_ASSIGNMENT (  '', '', ( #8732 ) ) ;
#10603 = CARTESIAN_POINT ( 'NONE',  ( 42.63976443033212860, 56.00051614449765935, -0.02388180880514948964 ) ) ;
#10604 = EDGE_CURVE ( 'NONE', #11691, #737, #18501, .T. ) ;
#10605 = CIRCLE ( 'NONE', #1533, 0.9999999999999982236 ) ;
#10606 = CARTESIAN_POINT ( 'NONE',  ( -74.99999999999997158, -1.000000000000000000, -5.999999999999998224 ) ) ;
#10607 = EDGE_LOOP ( 'NONE', ( #13413, #2935, #18639 ) ) ;
#10608 = CARTESIAN_POINT ( 'NONE',  ( 6.403457969954085449, 2.888443235695447253, -5.002930439003170804 ) ) ;
#10609 = VERTEX_POINT ( 'NONE', #13864 ) ;
#10610 = FACE_OUTER_BOUND ( 'NONE', #19159, .T. ) ;
#10611 = AXIS2_PLACEMENT_3D ( 'NONE', #16420, #227, #15126 ) ;
#10612 = CIRCLE ( 'NONE', #2814, 2.649999999999988365 ) ;
#10613 = CARTESIAN_POINT ( 'NONE',  ( 47.70284917648453415, 61.39948385550241738, -6.992620115222774047 ) ) ;
#10614 = DIRECTION ( 'NONE',  ( 0.000000000000000000, 0.000000000000000000, 1.000000000000000000 ) ) ;
#10615 = ORIENTED_EDGE ( 'NONE', *, *, #2638, .T. ) ;
#10616 = FACE_OUTER_BOUND ( 'NONE', #18312, .T. ) ;
#10617 = CARTESIAN_POINT ( 'NONE',  ( 2.449293598294706513E-15, -20.00000000000000000, -9.000000000000000000 ) ) ;
#10618 = CARTESIAN_POINT ( 'NONE',  ( 44.30067958973596376, 56.89948385550240317, 1.875703265242204099 ) ) ;
#10619 = PLANE ( 'NONE',  #13081 ) ;
#10620 = FACE_OUTER_BOUND ( 'NONE', #6355, .T. ) ;
#10621 = AXIS2_PLACEMENT_3D ( 'NONE', #11677, #4233, #17680 ) ;
#10622 = CARTESIAN_POINT ( 'NONE',  ( 42.39856655714564226, 54.10051614449766078, -2.493737253992044156 ) ) ;
#10623 = CARTESIAN_POINT ( 'NONE',  ( 53.54508667620424234, 54.70051614449765509, -4.840751629271188961 ) ) ;
#10624 = CARTESIAN_POINT ( 'NONE',  ( -6.473970235329672780E-16, -4.862606272033106691, -3.745885042887442395 ) ) ;
#10625 = LINE ( 'NONE', #18008, #6882 ) ;
#10626 = TOROIDAL_SURFACE ( 'NONE', #17539, 5.899999999999999467, 0.1000000000000010186 ) ;
#10627 = ORIENTED_EDGE ( 'NONE', *, *, #9498, .T. ) ;
#10628 = B_SPLINE_CURVE_WITH_KNOTS ( 'NONE', 3,
 ( #18415, #549, #14256, #12698, #18701, #6814, #18800, #9360, #15354, #646, #3500, #1939, #4956, #17034, #13873, #455 ),
 .UNSPECIFIED., .F., .F.,
 ( 4, 3, 3, 3, 3, 4 ),
 ( -2.111273352581767125E-06, 0.000000000000000000, 3.519286887793215919E-05, 7.191842652067064129E-05, 0.0001049868727093590168, 0.0001382836236822123786 ),
 .UNSPECIFIED. ) ;
#10629 = VERTEX_POINT ( 'NONE', #538 ) ;
#10630 = CARTESIAN_POINT ( 'NONE',  ( 7.900000000000002132, 0.000000000000000000, 0.000000000000000000 ) ) ;
#10631 = ORIENTED_EDGE ( 'NONE', *, *, #6386, .F. ) ;
#10632 = EDGE_CURVE ( 'NONE', #13559, #1748, #3490, .T. ) ;
#10633 = DIRECTION ( 'NONE',  ( 1.000000000000000000, 0.000000000000000000, 0.000000000000000000 ) ) ;
#10634 = DIRECTION ( 'NONE',  ( 1.000000000000000000, 0.000000000000000000, 0.000000000000000000 ) ) ;
#10635 = VECTOR ( 'NONE', #15194, 1000.000000000000000 ) ;
#10636 = VERTEX_POINT ( 'NONE', #11019 ) ;
#10637 = DIRECTION ( 'NONE',  ( 0.000000000000000000, -0.000000000000000000, 1.000000000000000000 ) ) ;
#10638 = EDGE_CURVE ( 'NONE', #16268, #15764, #19136, .T. ) ;
#10639 = CARTESIAN_POINT ( 'NONE',  ( 44.03140696652193498, 47.19948385550240744, -4.306917132069424170 ) ) ;
#10640 = ORIENTED_EDGE ( 'NONE', *, *, #7370, .T. ) ;
#10641 = CARTESIAN_POINT ( 'NONE',  ( -19.76107906696391225, -16.91783288752853665, -9.000000000000000000 ) ) ;
#10642 = ORIENTED_EDGE ( 'NONE', *, *, #12215, .F. ) ;
#10643 = CARTESIAN_POINT ( 'NONE',  ( 57.61547081786810764, 62.90051614449765083, -2.450534656007114176 ) ) ;
#10644 = CARTESIAN_POINT ( 'NONE',  ( 2.449293598294706513E-15, -20.00000000000000000, -9.999999999999994671 ) ) ;
#10645 = CARTESIAN_POINT ( 'NONE',  ( 55.94051828345050836, 57.79948385550238754, -4.345558710429104465 ) ) ;
#10646 = FACE_OUTER_BOUND ( 'NONE', #15803, .T. ) ;
#10647 = AXIS2_PLACEMENT_3D ( 'NONE', #8827, #10575, #16681 ) ;
#10648 = CONICAL_SURFACE ( 'NONE', #3770, 5.000000000000000000, 1.047197551196600296 ) ;
#10649 = CARTESIAN_POINT ( 'NONE',  ( 55.94051828345053679, 57.20051614449766930, 4.345558710429044069 ) ) ;
#10650 = CARTESIAN_POINT ( 'NONE',  ( 20.00000000000000000, -20.00000000000000000, -20.00000000000000000 ) ) ;
#10651 = AXIS2_PLACEMENT_3D ( 'NONE', #14165, #4177, #5539 ) ;
#10652 = CARTESIAN_POINT ( 'NONE',  ( 3.260336594487419859, -23.79080536174652494, -9.999999999999994671 ) ) ;
#10653 = ORIENTED_EDGE ( 'NONE', *, *, #8244, .T. ) ;
#10654 = EDGE_LOOP ( 'NONE', ( #16617, #12620, #2984, #7483 ) ) ;
#10655 =( REPRESENTATION_RELATIONSHIP ('NONE','NONE', #16703, #17450 ) REPRESENTATION_RELATIONSHIP_WITH_TRANSFORMATION ( #15584 )SHAPE_REPRESENTATION_RELATIONSHIP( ) );
#10656 = EDGE_LOOP ( 'NONE', ( #833, #4372, #9813, #14583 ) ) ;
#10657 = DIRECTION ( 'NONE',  ( 0.000000000000000000, 0.000000000000000000, 1.000000000000000000 ) ) ;
#10658 = FILL_AREA_STYLE_COLOUR ( '', #14997 ) ;
#10659 = VECTOR ( 'NONE', #1762, 1000.000000000000114 ) ;
#10660 = CARTESIAN_POINT ( 'NONE',  ( 45.86712807150323812, 47.29948385550240886, -5.649768623646098220 ) ) ;
#10661 = LINE ( 'NONE', #15460, #17834 ) ;
#10662 = VECTOR ( 'NONE', #4713, 1000.000000000000000 ) ;
#10663 = ORIENTED_EDGE ( 'NONE', *, *, #13576, .F. ) ;
#10664 = CYLINDRICAL_SURFACE ( 'NONE', #5500, 20.00000000000000000 ) ;
#10665 = AXIS2_PLACEMENT_3D ( 'NONE', #16118, #11780, #7477 ) ;
#10666 = EDGE_LOOP ( 'NONE', ( #18244, #9489, #18144, #1195 ) ) ;
#10667 = CARTESIAN_POINT ( 'NONE',  ( 50.02271294988505446, 56.50051614449766646, -7.000000000000000888 ) ) ;
#10668 = ORIENTED_EDGE ( 'NONE', *, *, #5822, .F. ) ;
#10669 = CARTESIAN_POINT ( 'NONE',  ( 6.445127866599364097, -3.194847394660946360, 4.687657648742338701 ) ) ;
#10670 = UNCERTAINTY_MEASURE_WITH_UNIT (LENGTH_MEASURE( 1.000000000000000082E-05 ), #12129, 'distance_accuracy_value', 'NONE');
#10671 = DIRECTION ( 'NONE',  ( 0.000000000000000000, 0.000000000000000000, -1.000000000000000000 ) ) ;
#10673 = AXIS2_PLACEMENT_3D ( 'NONE', #6543, #14183, #6645 ) ;
#10672 = CARTESIAN_POINT ( 'NONE',  ( 46.45491332379576477, 53.70051614449766220, 4.840751629271188961 ) ) ;
#10674 = DIRECTION ( 'NONE',  ( -1.000000000000000000, 0.000000000000000000, -0.000000000000000000 ) ) ;
#10675 = CARTESIAN_POINT ( 'NONE',  ( 55.08986747509847248, 59.79948385550240175, -3.727524721679197572 ) ) ;
#10676 = CARTESIAN_POINT ( 'NONE',  ( -19.30627432446643610, -25.22185519795866782, -9.000000000000000000 ) ) ;
#10677 = AXIS2_PLACEMENT_3D ( 'NONE', #2646, #8511, #14481 ) ;
#10678 = AXIS2_PLACEMENT_3D ( 'NONE', #6600, #18592, #13330 ) ;
#10679 = CARTESIAN_POINT ( 'NONE',  ( 57.60143344285435774, 55.10051614449765367, 2.493737253992045044 ) ) ;
#10680 = LINE ( 'NONE', #16683, #10635 ) ;
#10681 = ORIENTED_EDGE ( 'NONE', *, *, #3423, .F. ) ;
#10682 = DIRECTION ( 'NONE',  ( 1.000000000000000000, 0.000000000000000000, 0.000000000000000000 ) ) ;
#10683 = DIRECTION ( 'NONE',  ( 0.000000000000000000, 0.000000000000000000, 1.000000000000000000 ) ) ;
#10684 = EDGE_CURVE ( 'NONE', #2700, #9693, #8140, .T. ) ;
#10685 = DIRECTION ( 'NONE',  ( 0.000000000000000000, 0.000000000000000000, -1.000000000000000000 ) ) ;
#10686 = APPLICATION_PROTOCOL_DEFINITION ( 'draft international standard', 'automotive_design', 1998, #13257 ) ;
#10687 = ORIENTED_EDGE ( 'NONE', *, *, #5559, .F. ) ;
#10688 = LINE ( 'NONE', #9215, #804 ) ;
#10689 = CARTESIAN_POINT ( 'NONE',  ( -3.734041964264191549, -23.01611183630746638, -9.999999999999994671 ) ) ;
#10690 = AXIS2_PLACEMENT_3D ( 'NONE', #13775, #6335, #3394 ) ;
#10691 = VECTOR ( 'NONE', #6198, 1000.000000000000000 ) ;
#10692 = CARTESIAN_POINT ( 'NONE',  ( 52.25172492374522903, 61.59948385550239891, -7.007379884777227730 ) ) ;
#10693 = AXIS2_PLACEMENT_3D ( 'NONE', #15452, #4693, #13876 ) ;
#10694 = CARTESIAN_POINT ( 'NONE',  ( 20.00000000000000000, -20.00000000000000000, -23.00000000000000000 ) ) ;
#10695 = DIRECTION ( 'NONE',  ( 0.000000000000000000, 0.000000000000000000, 1.000000000000000000 ) ) ;
#10696 = CARTESIAN_POINT ( 'NONE',  ( 4.200000000000001954, 0.000000000000000000, 0.000000000000000000 ) ) ;
#10697 = CARTESIAN_POINT ( 'NONE',  ( 56.65037692655918988, 59.89948385550241028, -2.184720259617163762 ) ) ;
#10698 = EDGE_CURVE ( 'NONE', #3553, #3573, #5340, .T. ) ;
#10699 = CARTESIAN_POINT ( 'NONE',  ( -150.9999999999999716, -14.99999999999999645, 10.00000000000000000 ) ) ;
#10700 = CARTESIAN_POINT ( 'NONE',  ( 45.31609314410967926, 58.69948385550240033, 6.485486291978119766 ) ) ;
#10701 = CARTESIAN_POINT ( 'NONE',  ( 3.974175853610014908, -2.726149789692841274, -2.409821656223155806 ) ) ;
#10702 = CARTESIAN_POINT ( 'NONE',  ( 55.96859303347802239, 54.80051614449764230, -4.306917132069484566 ) ) ;
#10703 = LINE ( 'NONE', #4830, #13787 ) ;
#10704 = EDGE_CURVE ( 'NONE', #8542, #4201, #16008, .T. ) ;
#10705 = EDGE_CURVE ( 'NONE', #18844, #16440, #9101, .T. ) ;
#10706 = EDGE_CURVE ( 'NONE', #6580, #5943, #1610, .T. ) ;
#10707 = ORIENTED_EDGE ( 'NONE', *, *, #5375, .F. ) ;
#10708 = EDGE_CURVE ( 'NONE', #228, #6680, #12234, .T. ) ;
#10709 = CARTESIAN_POINT ( 'NONE',  ( 1.411581201560190495E-15, 4.862606272033091592, -3.745885042887436622 ) ) ;
#10710 = CARTESIAN_POINT ( 'NONE',  ( 55.94051828345054389, 49.20051614449766220, 4.345558710429044957 ) ) ;
#10711 = EDGE_CURVE ( 'NONE', #6643, #5237, #18691, .T. ) ;
#10712 = DIRECTION ( 'NONE',  ( -0.5000000000000041078, 0.8660254037844362651, 0.000000000000000000 ) ) ;
#10713 = AXIS2_PLACEMENT_3D ( 'NONE', #19397, #5935, #17906 ) ;
#10714 = CARTESIAN_POINT ( 'NONE',  ( 75.00000000000002842, -1.000000000000000000, -5.999999999999998224 ) ) ;
#10715 = ORIENTED_EDGE ( 'NONE', *, *, #2938, .T. ) ;
#10716 = CARTESIAN_POINT ( 'NONE',  ( -5.130877905917283321, -0.6693483836015013955, 9.000000000000000000 ) ) ;
#10717 = DIRECTION ( 'NONE',  ( -0.000000000000000000, -0.000000000000000000, -1.000000000000000000 ) ) ;
#10718 = CARTESIAN_POINT ( 'NONE',  ( 55.71335778527780747, 62.09948385550240602, 1.832500667257165983 ) ) ;
#10719 = DIRECTION ( 'NONE',  ( 0.000000000000000000, 0.000000000000000000, -1.000000000000000000 ) ) ;
#10720 = CYLINDRICAL_SURFACE ( 'NONE', #7355, 4.000000000000003553 ) ;
#10721 = CARTESIAN_POINT ( 'NONE',  ( 47.42335538002180328, 56.40051614449765793, -8.007379884777206414 ) ) ;
#10722 = CARTESIAN_POINT ( 'NONE',  ( 55.08986747509849380, 57.20051614449766220, 3.727524721679155384 ) ) ;
#10723 = CARTESIAN_POINT ( 'NONE',  ( 4.211140560182196957, -2.431303136016555122, -3.745885042887436622 ) ) ;
#10724 = FACE_OUTER_BOUND ( 'NONE', #7228, .T. ) ;
#10726 = ORIENTED_EDGE ( 'NONE', *, *, #13125, .T. ) ;
#10725 = ADVANCED_FACE ( 'NONE', ( #6802 ), #5234, .T. ) ;
#10727 = ADVANCED_FACE ( 'NONE', ( #8367 ), #14345, .F. ) ;
#10728 = ORIENTED_EDGE ( 'NONE', *, *, #19236, .F. ) ;
#10729 = DIRECTION ( 'NONE',  ( -0.000000000000000000, -0.000000000000000000, 1.000000000000000000 ) ) ;
#10730 = ORIENTED_EDGE ( 'NONE', *, *, #14539, .F. ) ;
#10731 = DIRECTION ( 'NONE',  ( -1.000000000000000000, 9.251858538542972814E-17, -0.000000000000000000 ) ) ;
#10732 = VECTOR ( 'NONE', #2112, 1000.000000000000000 ) ;
#10733 = ORIENTED_EDGE ( 'NONE', *, *, #17722, .T. ) ;
#10734 = CARTESIAN_POINT ( 'NONE',  ( -44.99999999999997158, -40.00000000000000000, -10.00000000000000000 ) ) ;
#10735 = CARTESIAN_POINT ( 'NONE',  ( 50.02271294988512551, 50.49948385550240459, 7.000000000000000888 ) ) ;
#10736 = VERTEX_POINT ( 'NONE', #17409 ) ;
#10737 = CARTESIAN_POINT ( 'NONE',  ( 0.000000000000000000, 0.000000000000000000, -4.484454397937119197 ) ) ;
#10738 = EDGE_LOOP ( 'NONE', ( #17524, #15585 ) ) ;
#10739 = CARTESIAN_POINT ( 'NONE',  ( 57.60143344285433642, 47.89948385550240317, -2.493737253992118319 ) ) ;
#10740 = DIRECTION ( 'NONE',  ( 0.000000000000000000, -0.000000000000000000, 1.000000000000000000 ) ) ;
#10741 = CARTESIAN_POINT ( 'NONE',  ( 45.86712807150323812, 59.29948385550240175, -5.649768623646098220 ) ) ;
#10742 = CARTESIAN_POINT ( 'NONE',  ( 6.371919382990604674, 1.972754410575522588, 5.108792907957607099 ) ) ;
#10743 = SURFACE_STYLE_USAGE ( .BOTH. , #10837 ) ;
#10744 = CARTESIAN_POINT ( 'NONE',  ( 49.97728705011495265, 57.50051614449766646, 7.000000000000000888 ) ) ;
#10745 = CARTESIAN_POINT ( 'NONE',  ( 52.80949999999998568, 0.000000000000000000, 0.000000000000000000 ) ) ;
#10746 = CARTESIAN_POINT ( 'NONE',  ( 47.74827507625478518, 52.59948385550239180, 7.007379884777227730 ) ) ;
#10747 = DIRECTION ( 'NONE',  ( 1.000000000000000000, -0.000000000000000000, -0.000000000000000000 ) ) ;
#10748 = ORIENTED_EDGE ( 'NONE', *, *, #6883, .F. ) ;
#10749 = EDGE_CURVE ( 'NONE', #16421, #10468, #9831, .T. ) ;
#10750 = EDGE_CURVE ( 'NONE', #17750, #7321, #4164, .T. ) ;
#10751 = VERTEX_POINT ( 'NONE', #2416 ) ;
#10752 = ORIENTED_EDGE ( 'NONE', *, *, #10684, .F. ) ;
#10753 = DIRECTION ( 'NONE',  ( 1.000000000000000000, 0.000000000000000000, 0.000000000000000000 ) ) ;
#10754 =( NAMED_UNIT ( * ) SI_UNIT ( $, .STERADIAN. ) SOLID_ANGLE_UNIT ( ) );
#10755 = VECTOR ( 'NONE', #9748, 1000.000000000000000 ) ;
#10756 = ADVANCED_FACE ( 'NONE', ( #929, #16128, #3968 ), #6901, .T. ) ;
#10757 = CARTESIAN_POINT ( 'NONE',  ( 43.34962307344081012, 54.89948385550240317, 2.184720259617164650 ) ) ;
#10758 = CARTESIAN_POINT ( 'NONE',  ( 19.89043790736544892, -17.90943073464672608, -9.000000000000000000 ) ) ;
#10759 = ORIENTED_EDGE ( 'NONE', *, *, #7370, .F. ) ;
#10760 = DIRECTION ( 'NONE',  ( -0.9781476007338035794, -0.2079116908177690293, 0.000000000000000000 ) ) ;
#10761 = ORIENTED_EDGE ( 'NONE', *, *, #2088, .T. ) ;
#10762 = CARTESIAN_POINT ( 'NONE',  ( 55.96859303347802239, 60.80051614449765651, -4.306917132069484566 ) ) ;
#10763 = ORIENTED_EDGE ( 'NONE', *, *, #10566, .T. ) ;
#10764 = CARTESIAN_POINT ( 'NONE',  ( 7.211304515372446211, -1.345319965580511479, 9.000000000000000000 ) ) ;
#10765 = CARTESIAN_POINT ( 'NONE',  ( 4.000000000000000000, 0.000000000000000000, 0.000000000000000000 ) ) ;
#10766 = CARTESIAN_POINT ( 'NONE',  ( 48.02776887271750184, 57.60051614449765367, 5.992620115222795363 ) ) ;
#10767 = DIRECTION ( 'NONE',  ( 0.000000000000000000, 0.000000000000000000, 1.000000000000000000 ) ) ;
#10768 = ADVANCED_FACE ( 'NONE', ( #9931 ), #12554, .F. ) ;
#10769 = CIRCLE ( 'NONE', #18001, 4.100000000000000533 ) ;
#10770 = CARTESIAN_POINT ( 'NONE',  ( -4.878909776184767981E-16, 0.4887495715076933811, 4.999999999999999112 ) ) ;
#10771 = CARTESIAN_POINT ( 'NONE',  ( 55.69932041026405045, 45.10051614449766788, 1.875703265242156359 ) ) ;
#10772 = DIRECTION ( 'NONE',  ( -1.000000000000000000, -0.000000000000000000, -0.000000000000000000 ) ) ;
#10773 = CARTESIAN_POINT ( 'NONE',  ( 58.41169779390614281, 53.00051614449765935, 0.02388180880515032231 ) ) ;
#10774 = EDGE_CURVE ( 'NONE', #162, #10751, #147, .T. ) ;
#10775 = VERTEX_POINT ( 'NONE', #10033 ) ;
#10776 = CYLINDRICAL_SURFACE ( 'NONE', #17497, 20.00000000000000000 ) ;
#10777 = ORIENTED_EDGE ( 'NONE', *, *, #9854, .T. ) ;
#10778 = DIRECTION ( 'NONE',  ( -1.000000000000000000, -0.000000000000000000, -0.000000000000000000 ) ) ;
#10779 = ORIENTED_EDGE ( 'NONE', *, *, #14905, .F. ) ;
#10780 = DIRECTION ( 'NONE',  ( 0.000000000000000000, 0.000000000000000000, 1.000000000000000000 ) ) ;
#10781 = CARTESIAN_POINT ( 'NONE',  ( 1.566204647097437341, -6.822536405429464601, -0.8000000000000000444 ) ) ;
#10782 = AXIS2_PLACEMENT_3D ( 'NONE', #16386, #11851, #9113 ) ;
#10783 = CARTESIAN_POINT ( 'NONE',  ( -54.99999999999996447, -14.99999999999998579, 15.00000000000000000 ) ) ;
#10784 = CARTESIAN_POINT ( 'NONE',  ( -59.84999999999998721, 32.50000000000001421, 15.00000000000000178 ) ) ;
#10785 = DIRECTION ( 'NONE',  ( 0.000000000000000000, 0.000000000000000000, 1.000000000000000000 ) ) ;
#10786 = CARTESIAN_POINT ( 'NONE',  ( -3.510273485745307287, -2.827716139362669967, -3.610536846335890004 ) ) ;
#10787 = CARTESIAN_POINT ( 'NONE',  ( 44.88205777487398507, 47.19948385550240744, -3.688883143319540814 ) ) ;
#10788 = CARTESIAN_POINT ( 'NONE',  ( 6.534838248920897819, 2.951765777552412651, 5.112608298763836601 ) ) ;
#10789 = CARTESIAN_POINT ( 'NONE',  ( 54.68390685589033495, 59.69948385550240744, -6.485486291978119766 ) ) ;
#10790 = CARTESIAN_POINT ( 'NONE',  ( 56.66441430157294690, 56.90051614449766504, -2.141517661632166281 ) ) ;
#10791 = CARTESIAN_POINT ( 'NONE',  ( -154.9999999999999716, -14.99999999999999645, 15.79999999999999893 ) ) ;
#10792 = CARTESIAN_POINT ( 'NONE',  ( -74.99999999999997158, 40.00000000000001421, -10.00000000000000000 ) ) ;
#10793 = CIRCLE ( 'NONE', #6403, 0.5999999999999980904 ) ;
#10794 = SURFACE_STYLE_FILL_AREA ( #18573 ) ;
#10795 = ORIENTED_EDGE ( 'NONE', *, *, #14178, .F. ) ;
#10796 = CIRCLE ( 'NONE', #7369, 0.5155456020628804703 ) ;
#10797 = CARTESIAN_POINT ( 'NONE',  ( 2.548804901056335857E-15, 4.736522675502163437, -3.681124513963624612 ) ) ;
#10798 = CARTESIAN_POINT ( 'NONE',  ( 52.25172492374528588, 47.40051614449765793, 7.007379884777204637 ) ) ;
#10799 = FACE_OUTER_BOUND ( 'NONE', #19387, .T. ) ;
#10800 = DIRECTION ( 'NONE',  ( -0.000000000000000000, -0.000000000000000000, 1.000000000000000000 ) ) ;
#10801 = ORIENTED_EDGE ( 'NONE', *, *, #8483, .T. ) ;
#10802 = CYLINDRICAL_SURFACE ( 'NONE', #19021, 4.799999999999999822 ) ;
#10803 = CARTESIAN_POINT ( 'NONE',  ( -3.175194142252083296, -39.74634503291706267, 9.000000000000000000 ) ) ;
#10804 = EDGE_CURVE ( 'NONE', #3235, #6953, #8487, .T. ) ;
#10805 = CARTESIAN_POINT ( 'NONE',  ( 49.97728705011494554, 45.50051614449766646, 6.000000000000000888 ) ) ;
#10806 = LINE ( 'NONE', #16810, #18739 ) ;
#10807 = CARTESIAN_POINT ( 'NONE',  ( 49.97728705011495265, 57.50051614449766646, 8.000000000000001776 ) ) ;
#10808 = PRODUCT_RELATED_PRODUCT_CATEGORY ( 'part', '', ( #11148 ) ) ;
#10809 = CIRCLE ( 'NONE', #6757, 0.5999999999999999778 ) ;
#10810 = CARTESIAN_POINT ( 'NONE',  ( 55.71335778527780036, 52.90051614449766504, -1.832500667257213056 ) ) ;
#10811 = EDGE_CURVE ( 'NONE', #3485, #9785, #15052, .T. ) ;
#10812 = DIRECTION ( 'NONE',  ( 0.000000000000000000, 0.000000000000000000, 1.000000000000000000 ) ) ;
#10813 = FACE_OUTER_BOUND ( 'NONE', #2893, .T. ) ;
#10814 = VERTEX_POINT ( 'NONE', #10512 ) ;
#10815 = ADVANCED_FACE ( 'NONE', ( #1415 ), #10221, .F. ) ;
#10816 = ADVANCED_FACE ( 'NONE', ( #1513 ), #17797, .F. ) ;
#10817 = CIRCLE ( 'NONE', #10509, 9.999999999999998224 ) ;
#10818 = EDGE_LOOP ( 'NONE', ( #10027, #11495, #7842, #2334 ) ) ;
#10819 = CARTESIAN_POINT ( 'NONE',  ( 14.14213562373094923, -14.99999999999999112, -20.00000000000000000 ) ) ;
#10820 = EDGE_LOOP ( 'NONE', ( #15924, #7817, #12342, #10514 ) ) ;
#10821 = EDGE_CURVE ( 'NONE', #15249, #15436, #15369, .T. ) ;
#10822 = CARTESIAN_POINT ( 'NONE',  ( 62.50000000000000000, 20.00000000000001421, 15.00000000000000000 ) ) ;
#10823 = VERTEX_POINT ( 'NONE', #11694 ) ;
#10824 = DIRECTION ( 'NONE',  ( -1.000000000000000000, 0.000000000000000000, 0.000000000000000000 ) ) ;
#10825 = VECTOR ( 'NONE', #9957, 1000.000000000000000 ) ;
#10826 = CARTESIAN_POINT ( 'NONE',  ( 45.90387839640214196, 54.69948385550240744, 5.676469297603166098 ) ) ;
#10827 = VERTEX_POINT ( 'NONE', #4553 ) ;
#10828 = DIRECTION ( 'NONE',  ( -0.000000000000000000, -0.000000000000000000, -1.000000000000000000 ) ) ;
#10829 = ORIENTED_EDGE ( 'NONE', *, *, #295, .F. ) ;
#10830 = CARTESIAN_POINT ( 'NONE',  ( 42.38452918213188525, 49.09948385550241312, -2.450534656007040013 ) ) ;
#10831 = FACE_OUTER_BOUND ( 'NONE', #5333, .T. ) ;
#10832 = ADVANCED_FACE ( 'NONE', ( #2797 ), #1917, .T. ) ;
#10833 = CARTESIAN_POINT ( 'NONE',  ( 49.97728705011488159, 63.49948385550241170, -7.000000000000000888 ) ) ;
#10834 = CARTESIAN_POINT ( 'NONE',  ( 0.000000000000000000, 0.000000000000000000, -0.3080913168122742518 ) ) ;
#10835 = CIRCLE ( 'NONE', #6146, 20.00000000000000000 ) ;
#10836 = EDGE_CURVE ( 'NONE', #18521, #18734, #19285, .T. ) ;
#10837 = SURFACE_SIDE_STYLE ('',( #16655 ) ) ;
#10838 = CARTESIAN_POINT ( 'NONE',  ( 56.66441430157294690, 62.90051614449765083, -2.141517661632166281 ) ) ;
#10839 = CARTESIAN_POINT ( 'NONE',  ( -2.688821387764050996E-14, -4.618802153517012954, -0.4999999999999995559 ) ) ;
#10840 = CARTESIAN_POINT ( 'NONE',  ( 55.94051828345050836, 49.79948385550240175, -4.345558710429104465 ) ) ;
#10841 = CARTESIAN_POINT ( 'NONE',  ( 6.436591462021358012, -5.789018756751932671, 5.527293451046372024E-16 ) ) ;
#10842 = VECTOR ( 'NONE', #14226, 1000.000000000000000 ) ;
#10843 = ORIENTED_EDGE ( 'NONE', *, *, #1377, .T. ) ;
#10844 = EDGE_LOOP ( 'NONE', ( #378, #8019, #8662, #14936 ) ) ;
#10845 = LINE ( 'NONE', #4968, #14989 ) ;
#10846 =( LENGTH_UNIT ( ) NAMED_UNIT ( * ) SI_UNIT ( .MILLI., .METRE. ) );
#10847 = CARTESIAN_POINT ( 'NONE',  ( 52.29715082351547295, 52.39948385550241738, 6.992620115222774047 ) ) ;
#10848 = ORIENTED_EDGE ( 'NONE', *, *, #17927, .T. ) ;
#10849 = DIRECTION ( 'NONE',  ( -0.000000000000000000, -0.000000000000000000, -1.000000000000000000 ) ) ;
#10850 = AXIS2_PLACEMENT_3D ( 'NONE', #13657, #12185, #2900 ) ;
#10851 = ORIENTED_EDGE ( 'NONE', *, *, #10481, .F. ) ;
#10852 = CARTESIAN_POINT ( 'NONE',  ( 0.000000000000000000, 0.000000000000000000, -0.2800830152838844622 ) ) ;
#10853 = ORIENTED_EDGE ( 'NONE', *, *, #8682, .T. ) ;
#10854 = AXIS2_PLACEMENT_3D ( 'NONE', #18540, #5372, #11343 ) ;
#10855 = CARTESIAN_POINT ( 'NONE',  ( 2.449293598294706513E-15, -20.00000000000000000, -9.000000000000000000 ) ) ;
#10856 = PRODUCT_DEFINITION_CONTEXT ( 'detailed design', #11024, 'design' ) ;
#10857 = LINE ( 'NONE', #101, #13365 ) ;
#10858 = CARTESIAN_POINT ( 'NONE',  ( 51.97223112728249816, 54.60051614449766788, -5.992620115222793586 ) ) ;
#10859 = FACE_OUTER_BOUND ( 'NONE', #9168, .T. ) ;
#10860 = VECTOR ( 'NONE', #5713, 1000.000000000000000 ) ;
#10861 = EDGE_CURVE ( 'NONE', #3030, #11109, #2233, .T. ) ;
#10862 = CARTESIAN_POINT ( 'NONE',  ( 0.000000000000000000, 0.000000000000000000, -4.974599999999998801 ) ) ;
#10863 = CARTESIAN_POINT ( 'NONE',  ( 57.60143344285435774, 61.10051614449766788, 2.493737253992045044 ) ) ;
#10864 = VECTOR ( 'NONE', #13124, 1000.000000000000000 ) ;
#10865 = EDGE_LOOP ( 'NONE', ( #8094, #10872, #7407 ) ) ;
#10866 = ORIENTED_EDGE ( 'NONE', *, *, #18396, .T. ) ;
#10867 = CARTESIAN_POINT ( 'NONE',  ( 0.000000000000000000, 0.000000000000000000, 0.000000000000000000 ) ) ;
#10868 = FILL_AREA_STYLE_COLOUR ( '', #4031 ) ;
#10869 = CIRCLE ( 'NONE', #5888, 4.100000000000000533 ) ;
#10870 = EDGE_LOOP ( 'NONE', ( #12445, #16515, #3093, #17973 ) ) ;
#10871 = CARTESIAN_POINT ( 'NONE',  ( -1.000000000000000000, -14.00000000000000000, 8.999999999999998224 ) ) ;
#10872 = ORIENTED_EDGE ( 'NONE', *, *, #6386, .T. ) ;
#10874 = LINE ( 'NONE', #9495, #17726 ) ;
#10873 = APPLICATION_CONTEXT ( 'automotive_design' ) ;
#10875 = EDGE_CURVE ( 'NONE', #9693, #15486, #4731, .T. ) ;
#10876 = CARTESIAN_POINT ( 'NONE',  ( 0.000000000000000000, 40.00000000000001421, 9.999999999999998224 ) ) ;
#10877 = AXIS2_PLACEMENT_3D ( 'NONE', #15018, #1597, #3260 ) ;
#10878 = ADVANCED_FACE ( 'NONE', ( #14838 ), #44, .T. ) ;
#10879 = AXIS2_PLACEMENT_3D ( 'NONE', #14212, #9803, #18858 ) ;
#10880 = CARTESIAN_POINT ( 'NONE',  ( 45.86712807150323812, 63.29948385550240886, -5.649768623646098220 ) ) ;
#10881 = DIRECTION ( 'NONE',  ( 0.9135454576426006446, 0.4067366430758008189, 0.000000000000000000 ) ) ;
#10882 = DIRECTION ( 'NONE',  ( -0.000000000000000000, 0.000000000000000000, -1.000000000000000000 ) ) ;
#10883 = FACE_OUTER_BOUND ( 'NONE', #12912, .T. ) ;
#10884 = CARTESIAN_POINT ( 'NONE',  ( 42.63976443033212860, 64.99948385550240459, 0.02388180880522514787 ) ) ;
#10885 = DIRECTION ( 'NONE',  ( -1.387778780781445676E-16, 1.000000000000000000, 0.000000000000000000 ) ) ;
#10886 = CARTESIAN_POINT ( 'NONE',  ( 43.20883090819745576, 62.79948385550240175, 4.963592699179006473 ) ) ;
#10887 = CARTESIAN_POINT ( 'NONE',  ( 56.65037692655921120, 63.10051614449766078, 2.184720259617097593 ) ) ;
#10888 = DIRECTION ( 'NONE',  ( -0.000000000000000000, -0.000000000000000000, -1.000000000000000000 ) ) ;
#10889 = DIRECTION ( 'NONE',  ( 1.000000000000000000, 0.000000000000000000, 0.000000000000000000 ) ) ;
#10890 = AXIS2_PLACEMENT_3D ( 'NONE', #3918, #13516, #5870 ) ;
#10891 = SHAPE_REPRESENTATION_RELATIONSHIP ( 'NONE' , 'NONE' ,  #14681, #1480 ) ;
#10892 = VERTEX_POINT ( 'NONE', #14935 ) ;
#10893 = DIRECTION ( 'NONE',  ( -1.000000000000000000, -0.000000000000000000, -0.000000000000000000 ) ) ;
#10894 = DIRECTION ( 'NONE',  ( -1.000000000000000000, -0.000000000000000000, -0.000000000000000000 ) ) ;
#10895 = CARTESIAN_POINT ( 'NONE',  ( 44.05948171654949874, 62.79948385550241596, 4.345558710429105354 ) ) ;
#10896 = CARTESIAN_POINT ( 'NONE',  ( -1.150000000000001688, 7.347880794884120722E-16, 6.000000000000001776 ) ) ;
#10897 = ORIENTED_EDGE ( 'NONE', *, *, #13111, .F. ) ;
#10898 = DIRECTION ( 'NONE',  ( 1.000000000000000000, 0.000000000000000000, 0.000000000000000000 ) ) ;
#10899 = B_SPLINE_CURVE_WITH_KNOTS ( 'NONE', 3,
 ( #1498, #11775, #12171, #6016, #19371 ),
 .UNSPECIFIED., .F., .F.,
 ( 4, 1, 4 ),
 ( 0.000000000000000000, 0.002309401076758505790, 0.004618802153517011580 ),
 .UNSPECIFIED. ) ;
#10900 = VECTOR ( 'NONE', #11133, 1000.000000000000114 ) ;
#10901 = DIRECTION ( 'NONE',  ( 1.000000000000000000, 0.000000000000000000, 0.000000000000000000 ) ) ;
#10902 = CARTESIAN_POINT ( 'NONE',  ( 55.69932041026404335, 61.89948385550241738, -1.875703265242203432 ) ) ;
#10903 = CARTESIAN_POINT ( 'NONE',  ( -151.2001253019789431, -14.96914097636792818, 15.79999999999999893 ) ) ;
#10904 = CARTESIAN_POINT ( 'NONE',  ( 54.13287192849676188, 48.29948385550240175, 5.649768623646098220 ) ) ;
#10905 = CARTESIAN_POINT ( 'NONE',  ( 3.973110223768737015, -0.6864646529411583264, -3.565797985667475078 ) ) ;
#10906 = CARTESIAN_POINT ( 'NONE',  ( 58.41169779390614281, 57.00051614449766646, 0.02388180880515032231 ) ) ;
#10907 = CARTESIAN_POINT ( 'NONE',  ( 53.50833635130544508, 55.30051614449765651, 4.867452303228181343 ) ) ;
#10908 =( GEOMETRIC_REPRESENTATION_CONTEXT ( 3 ) GLOBAL_UNCERTAINTY_ASSIGNED_CONTEXT ( ( #12049 ) ) GLOBAL_UNIT_ASSIGNED_CONTEXT ( ( #10080, #275, #1561 ) ) REPRESENTATION_CONTEXT ( 'NONE', 'WORKASPACE' ) );
#10909 = DIRECTION ( 'NONE',  ( -1.000000000000000000, 0.000000000000000000, 0.000000000000000000 ) ) ;
#10910 = CARTESIAN_POINT ( 'NONE',  ( 6.327632967271008546, -3.313549392874691524, -4.260764098152702850 ) ) ;
#10911 = ORIENTED_EDGE ( 'NONE', *, *, #6636, .F. ) ;
#10912 = ORIENTED_EDGE ( 'NONE', *, *, #7093, .T. ) ;
#10913 = LINE ( 'NONE', #16921, #17835 ) ;
#10914 = ORIENTED_EDGE ( 'NONE', *, *, #10960, .T. ) ;
#10915 = VECTOR ( 'NONE', #19189, 1000.000000000000000 ) ;
#10916 = ADVANCED_FACE ( 'NONE', ( #10610 ), #8950, .F. ) ;
#10917 = VECTOR ( 'NONE', #17503, 1000.000000000000114 ) ;
#10918 = CARTESIAN_POINT ( 'NONE',  ( 1.599999999999999867, -5.408326913195983465, 0.000000000000000000 ) ) ;
#10919 = EDGE_LOOP ( 'NONE', ( #10059, #13771, #4972, #9469 ) ) ;
#10920 = DIRECTION ( 'NONE',  ( 0.000000000000000000, 0.000000000000000000, -1.000000000000000000 ) ) ;
#10921 = CARTESIAN_POINT ( 'NONE',  ( 49.97728705011488159, 55.49948385550240459, -7.000000000000000888 ) ) ;
#10922 = VERTEX_POINT ( 'NONE', #5924 ) ;
#10923 = COLOUR_RGB ( '',0.8941176470588234615, 0.8941176470588234615, 0.8941176470588234615 ) ;
#10924 = DIRECTION ( 'NONE',  ( 0.000000000000000000, 0.000000000000000000, -1.000000000000000000 ) ) ;
#10925 = ORIENTED_EDGE ( 'NONE', *, *, #15633, .T. ) ;
#10926 = CARTESIAN_POINT ( 'NONE',  ( 47.42335538002188144, 50.59948385550240602, 8.007379884777233059 ) ) ;
#10927 = CARTESIAN_POINT ( 'NONE',  ( 4.030859730899086557, -1.403482646610860307, -3.500000000000000000 ) ) ;
#10928 = CARTESIAN_POINT ( 'NONE',  ( 49.97728705011488159, 65.49948385550240459, -7.000000000000000888 ) ) ;
#10929 = LINE ( 'NONE', #3592, #10407 ) ;
#10930 = CARTESIAN_POINT ( 'NONE',  ( 4.158413352280810216, -4.089743253945651524, 4.401844587977598791E-16 ) ) ;
#10931 = CARTESIAN_POINT ( 'NONE',  ( 45.86712807150329496, 63.70051614449766220, 5.649768623646139964 ) ) ;
#10932 = CIRCLE ( 'NONE', #15337, 4.000000000000031086 ) ;
#10933 = VECTOR ( 'NONE', #12255, 1000.000000000000000 ) ;
#10934 = CARTESIAN_POINT ( 'NONE',  ( -154.9999999999999716, -14.99999999999999645, -17.00000000000000000 ) ) ;
#10935 = EDGE_CURVE ( 'NONE', #12330, #7075, #16222, .T. ) ;
#10936 = CARTESIAN_POINT ( 'NONE',  ( 45.90387839640214196, 60.69948385550240033, 5.676469297603166098 ) ) ;
#10937 = DIRECTION ( 'NONE',  ( -1.000000000000000000, 0.000000000000000000, 0.000000000000000000 ) ) ;
#10938 = EDGE_LOOP ( 'NONE', ( #7252, #10370, #6686, #2317 ) ) ;
#10939 = CIRCLE ( 'NONE', #7510, 4.000000000000003553 ) ;
#10940 = VERTEX_POINT ( 'NONE', #11887 ) ;
#10941 = DIRECTION ( 'NONE',  ( 0.1305261922200524616, -0.9914448613738103822, 0.000000000000000000 ) ) ;
#10942 =( LENGTH_UNIT ( ) NAMED_UNIT ( * ) SI_UNIT ( .MILLI., .METRE. ) );
#10943 = EDGE_CURVE ( 'NONE', #9923, #10736, #1088, .T. ) ;
#10944 = CARTESIAN_POINT ( 'NONE',  ( 54.09612160359786515, 51.69948385550240744, -5.676469297603166098 ) ) ;
#10945 = EDGE_CURVE ( 'NONE', #11695, #3362, #15681, .T. ) ;
#10946 = DIRECTION ( 'NONE',  ( 0.3090169943749456194, 0.9510565162951541973, 0.000000000000000000 ) ) ;
#10947 = VERTEX_POINT ( 'NONE', #18091 ) ;
#10948 = DIRECTION ( 'NONE',  ( -0.000000000000000000, -0.000000000000000000, -1.000000000000000000 ) ) ;
#10949 = CIRCLE ( 'NONE', #2189, 4.800000000000000711 ) ;
#10950 = VERTEX_POINT ( 'NONE', #11990 ) ;
#10951 = CARTESIAN_POINT ( 'NONE',  ( -149.0000000000000000, -14.99999999999999645, -9.000000000000000000 ) ) ;
#10952 = ORIENTED_EDGE ( 'NONE', *, *, #9721, .F. ) ;
#10953 = EDGE_CURVE ( 'NONE', #8597, #1096, #649, .T. ) ;
#10954 = CARTESIAN_POINT ( 'NONE',  ( 52.25172492374522903, 45.59948385550240602, -7.007379884777225953 ) ) ;
#10955 = DIRECTION ( 'NONE',  ( 9.710251638871371392E-17, 5.969973981896233748E-17, 1.000000000000000000 ) ) ;
#10956 = VECTOR ( 'NONE', #2725, 1000.000000000000000 ) ;
#10957 = EDGE_CURVE ( 'NONE', #10814, #2113, #7551, .T. ) ;
#10958 = CARTESIAN_POINT ( 'NONE',  ( 55.71335778527780036, 60.90051614449766504, -1.832500667257213056 ) ) ;
#10959 = FACE_OUTER_BOUND ( 'NONE', #12735, .T. ) ;
#10960 = EDGE_CURVE ( 'NONE', #17786, #18623, #8860, .T. ) ;
#10961 = CARTESIAN_POINT ( 'NONE',  ( 1.925929944387235853E-31, 15.00000000000001599, 15.00000000000000000 ) ) ;
#10962 = LINE ( 'NONE', #9391, #9100 ) ;
#10963 = CIRCLE ( 'NONE', #4403, 5.400000000000000355 ) ;
#10964 = CARTESIAN_POINT ( 'NONE',  ( 58.41169779390614281, 59.00051614449766646, 0.02388180880515032231 ) ) ;
#10965 = AXIS2_PLACEMENT_3D ( 'NONE', #12630, #17062, #3524 ) ;
#10966 = CIRCLE ( 'NONE', #2550, 15.00000000000000000 ) ;
#10967 = ORIENTED_EDGE ( 'NONE', *, *, #10114, .F. ) ;
#10968 = ORIENTED_EDGE ( 'NONE', *, *, #2207, .F. ) ;
#10969 = CARTESIAN_POINT ( 'NONE',  ( 2.449293598294706513E-15, -20.00000000000000000, 9.999999999999998224 ) ) ;
#10970 = CARTESIAN_POINT ( 'NONE',  ( 2.321707774797442170, -4.824281976789052351, -0.8000000000000000444 ) ) ;
#10971 = CONTEXT_DEPENDENT_SHAPE_REPRESENTATION ( #10281, #1165 ) ;
#10972 = AXIS2_PLACEMENT_3D ( 'NONE', #18082, #18276, #12277 ) ;
#10973 = ORIENTED_EDGE ( 'NONE', *, *, #6658, .F. ) ;
#10974 = DIRECTION ( 'NONE',  ( 0.000000000000000000, -1.000000000000000000, 0.000000000000000000 ) ) ;
#10975 = CARTESIAN_POINT ( 'NONE',  ( -12.54977455159124133, -4.427487078052150693, 0.000000000000000000 ) ) ;
#10976 = VERTEX_POINT ( 'NONE', #1706 ) ;
#10977 = VECTOR ( 'NONE', #8228, 1000.000000000000000 ) ;
#10978 = CARTESIAN_POINT ( 'NONE',  ( -20.00000000000000000, -19.99999999999999289, -12.00000000000000000 ) ) ;
#10979 = AXIS2_PLACEMENT_3D ( 'NONE', #7920, #12030, #13214 ) ;
#10980 = CARTESIAN_POINT ( 'NONE',  ( 62.49999999999998579, 40.00000000000001421, -5.000000000000000000 ) ) ;
#10981 = AXIS2_PLACEMENT_3D ( 'NONE', #15035, #1617, #13562 ) ;
#10982 = AXIS2_PLACEMENT_3D ( 'NONE', #7971, #526, #15141 ) ;
#10983 = CARTESIAN_POINT ( 'NONE',  ( -54.99999999999996447, -14.99999999999998579, 15.00000000000000000 ) ) ;
#10984 = DIRECTION ( 'NONE',  ( -0.000000000000000000, 1.000000000000000000, -0.000000000000000000 ) ) ;
#10985 = CARTESIAN_POINT ( 'NONE',  ( 52.29715082351547295, 64.39948385550239607, 6.992620115222774047 ) ) ;
#10986 = DIRECTION ( 'NONE',  ( 0.000000000000000000, 0.000000000000000000, 1.000000000000000000 ) ) ;
#10987 = CARTESIAN_POINT ( 'NONE',  ( 42.39856655714566358, 56.89948385550240317, 2.493737253992119207 ) ) ;
#10988 = CARTESIAN_POINT ( 'NONE',  ( 56.65037692655921120, 61.10051614449766078, 2.184720259617097593 ) ) ;
#10989 = ADVANCED_FACE ( 'NONE', ( #333 ), #12538, .T. ) ;
#10990 = CARTESIAN_POINT ( 'NONE',  ( -154.9999999999999716, -14.99999999999999645, -6.499999999999999112 ) ) ;
#10991 = DIRECTION ( 'NONE',  ( -0.000000000000000000, -0.000000000000000000, 1.000000000000000000 ) ) ;
#10992 = EDGE_CURVE ( 'NONE', #870, #4952, #3652, .T. ) ;
#10993 = ORIENTED_EDGE ( 'NONE', *, *, #5800, .T. ) ;
#10994 = VECTOR ( 'NONE', #10986, 1000.000000000000000 ) ;
#10995 = VECTOR ( 'NONE', #9919, 1000.000000000000000 ) ;
#10996 = DIRECTION ( 'NONE',  ( -1.000000000000000000, 0.000000000000000000, 0.000000000000000000 ) ) ;
#10997 = DIRECTION ( 'NONE',  ( -0.000000000000000000, -0.000000000000000000, 1.000000000000000000 ) ) ;
#10998 = CARTESIAN_POINT ( 'NONE',  ( 32.00000000000000000, 1.000000000000000000, -5.999999999999998224 ) ) ;
#10999 = LINE ( 'NONE', #16711, #2107 ) ;
#11000 = ORIENTED_EDGE ( 'NONE', *, *, #7458, .T. ) ;
#11001 = DIRECTION ( 'NONE',  ( -9.710251638871371392E-17, -5.969973981896233748E-17, -1.000000000000000000 ) ) ;
#11002 = DIRECTION ( 'NONE',  ( 0.1305261922200524616, 0.9914448613738103822, -0.000000000000000000 ) ) ;
#11003 = B_SPLINE_CURVE_WITH_KNOTS ( 'NONE', 3,
 ( #8501, #755, #8592, #5362 ),
 .UNSPECIFIED., .F., .F.,
 ( 4, 4 ),
 ( 0.000000000000000000, 0.002080789711329271950 ),
 .UNSPECIFIED. ) ;
#11004 = CARTESIAN_POINT ( 'NONE',  ( 44.30067958973596376, 62.89948385550240317, 1.875703265242204099 ) ) ;
#11005 = CARTESIAN_POINT ( 'NONE',  ( -19.02113032590308705, -13.81966011250110249, 9.000000000000000000 ) ) ;
#11006 = CARTESIAN_POINT ( 'NONE',  ( 43.33558569842703179, 47.09948385550240602, -2.141517661632099223 ) ) ;
#11007 = CARTESIAN_POINT ( 'NONE',  ( -2.687328764639638656, 3.067272167851286202, -0.05923475698270370959 ) ) ;
#11008 = CARTESIAN_POINT ( 'NONE',  ( 47.42335538002180328, 62.40051614449765793, -8.007379884777206414 ) ) ;
#11009 = CARTESIAN_POINT ( 'NONE',  ( 56.65037692655921120, 45.10051614449766078, 2.184720259617097593 ) ) ;
#11010 = CIRCLE ( 'NONE', #5070, 20.00000000000000000 ) ;
#11011 = CARTESIAN_POINT ( 'NONE',  ( -154.9999999999999716, -23.00000000000000000, 10.00000000000000000 ) ) ;
#11012 = CARTESIAN_POINT ( 'NONE',  ( -4.688877333428352223, -21.02685410450703074, 9.000000000000000000 ) ) ;
#11013 = EDGE_LOOP ( 'NONE', ( #5581, #2269, #19289, #13765, #13745, #19404 ) ) ;
#11014 = EDGE_LOOP ( 'NONE', ( #14911, #11717, #16583, #18687 ) ) ;
#11015 = CARTESIAN_POINT ( 'NONE',  ( 62.49999999999998579, 32.50000000000001421, -9.999999999999998224 ) ) ;
#11016 = VERTEX_POINT ( 'NONE', #510 ) ;
#11017 = DIRECTION ( 'NONE',  ( -0.000000000000000000, 1.000000000000000000, -0.000000000000000000 ) ) ;
#11018 = ORIENTED_EDGE ( 'NONE', *, *, #13922, .F. ) ;
#11019 = CARTESIAN_POINT ( 'NONE',  ( -0.1085714285714285687, -3.798448662927795372, 0.000000000000000000 ) ) ;
#11020 = CARTESIAN_POINT ( 'NONE',  ( 42.63976443033212149, 54.99948385550239749, 0.02388180880522514787 ) ) ;
#11021 = ORIENTED_EDGE ( 'NONE', *, *, #16666, .F. ) ;
#11022 = FACE_OUTER_BOUND ( 'NONE', #7560, .T. ) ;
#11023 = ORIENTED_EDGE ( 'NONE', *, *, #17341, .T. ) ;
#11024 = APPLICATION_CONTEXT ( 'automotive_design' ) ;
#11025 = CARTESIAN_POINT ( 'NONE',  ( 43.18075615816989199, 53.19948385550240744, -4.924951120819313743 ) ) ;
#11026 = DIRECTION ( 'NONE',  ( 0.000000000000000000, 0.000000000000000000, 1.000000000000000000 ) ) ;
#11027 = CARTESIAN_POINT ( 'NONE',  ( 46.49166364869460466, 46.69948385550240744, 4.867452303228209765 ) ) ;
#11028 = CARTESIAN_POINT ( 'NONE',  ( -13.86289650954781649, -33.38261212717723936, -9.000000000000000000 ) ) ;
#11029 = CARTESIAN_POINT ( 'NONE',  ( -0.2000000000000000111, -6.997142273814360713, 0.000000000000000000 ) ) ;
#11030 = CARTESIAN_POINT ( 'NONE',  ( 43.34962307344078880, 62.10051614449766078, -2.184720259617096705 ) ) ;
#11031 = CARTESIAN_POINT ( 'NONE',  ( 42.63976443033212860, 58.99948385550239038, 0.02388180880522514787 ) ) ;
#11032 = CARTESIAN_POINT ( 'NONE',  ( 6.534224484704327374, -5.901860969583205829, 2.643887195172161483E-14 ) ) ;
#11033 = CARTESIAN_POINT ( 'NONE',  ( 32.49999999999998579, 45.00000000000001421, -4.999999999999996447 ) ) ;
#11034 = VERTEX_POINT ( 'NONE', #9613 ) ;
#11035 = PRODUCT_DEFINITION_FORMATION_WITH_SPECIFIED_SOURCE ( 'ANY', '', #11800, .NOT_KNOWN. ) ;
#11036 = EDGE_LOOP ( 'NONE', ( #17309, #825, #7889, #6002 ) ) ;
#11037 = CARTESIAN_POINT ( 'NONE',  ( -74.99999999999997158, -39.99999999999998579, -10.00000000000000000 ) ) ;
#11038 = FILL_AREA_STYLE_COLOUR ( '', #14038 ) ;
#11039 = CARTESIAN_POINT ( 'NONE',  ( 42.63976443033212860, 48.99948385550240459, 0.02388180880522514787 ) ) ;
#11040 = FACE_OUTER_BOUND ( 'NONE', #4787, .T. ) ;
#11041 = VERTEX_POINT ( 'NONE', #11086 ) ;
#11042 = EDGE_LOOP ( 'NONE', ( #16130, #15277, #3029, #11605 ) ) ;
#11043 = DIRECTION ( 'NONE',  ( 0.000000000000000000, 0.000000000000000000, 1.000000000000000000 ) ) ;
#11044 = EDGE_LOOP ( 'NONE', ( #6455, #8009, #471, #15505, #14688, #18870, #13860, #2758 ) ) ;
#11045 = ADVANCED_BREP_SHAPE_REPRESENTATION ( '', ( #2292, #10359 ), #11543 ) ;
#11046 = DIRECTION ( 'NONE',  ( 1.000000000000000000, 0.000000000000000000, 0.000000000000000000 ) ) ;
#11047 = ORIENTED_EDGE ( 'NONE', *, *, #7997, .T. ) ;
#11048 = CARTESIAN_POINT ( 'NONE',  ( 49.97728705011488159, 45.49948385550240459, -7.000000000000000888 ) ) ;
#11049 = PRODUCT_DEFINITION_CONTEXT ( 'detailed design', #9275, 'design' ) ;
#11050 = DIRECTION ( 'NONE',  ( 0.000000000000000000, 0.000000000000000000, 1.000000000000000000 ) ) ;
#11051 = CARTESIAN_POINT ( 'NONE',  ( 44.88205777487401349, 61.80051614449766362, 3.688883143319584779 ) ) ;
#11052 = DIRECTION ( 'NONE',  ( -2.191393683118470056E-17, -7.538405132783724027E-17, -1.000000000000000000 ) ) ;
#11053 = EDGE_CURVE ( 'NONE', #9631, #11812, #15313, .T. ) ;
#11054 = DIRECTION ( 'NONE',  ( 0.000000000000000000, 0.000000000000000000, 1.000000000000000000 ) ) ;
#11055 = CARTESIAN_POINT ( 'NONE',  ( 6.534838248920897819, 2.951765777552411318, -5.112608298763837489 ) ) ;
#11056 = CARTESIAN_POINT ( 'NONE',  ( 49.97728705011495265, 61.50051614449766646, 8.000000000000001776 ) ) ;
#11057 = EDGE_CURVE ( 'NONE', #178, #10922, #12422, .T. ) ;
#11058 = EDGE_LOOP ( 'NONE', ( #9572, #6631, #4040, #7716 ) ) ;
#11059 = ORIENTED_EDGE ( 'NONE', *, *, #12021, .T. ) ;
#11060 = DIRECTION ( 'NONE',  ( 0.000000000000000000, 0.000000000000000000, 1.000000000000000000 ) ) ;
#11061 = EDGE_CURVE ( 'NONE', #16758, #9546, #17052, .T. ) ;
#11062 = EDGE_CURVE ( 'NONE', #18720, #18478, #9414, .T. ) ;
#11063 = LINE ( 'NONE', #16779, #926 ) ;
#11064 = CONTEXT_DEPENDENT_SHAPE_REPRESENTATION ( #12292, #2904 ) ;
#11065 = VERTEX_POINT ( 'NONE', #9775 ) ;
#11066 = CARTESIAN_POINT ( 'NONE',  ( 2.449293598294706513E-15, -20.00000000000000000, 9.000000000000000000 ) ) ;
#11067 = EDGE_CURVE ( 'NONE', #7311, #2212, #5996, .T. ) ;
#11068 = CARTESIAN_POINT ( 'NONE',  ( 5.599999999999999645, 4.041451884327382338, 0.000000000000000000 ) ) ;
#11069 = EDGE_LOOP ( 'NONE', ( #131, #6164, #2853, #1366 ) ) ;
#11070 = CARTESIAN_POINT ( 'NONE',  ( -9.999999999999994671, 20.00000000000001421, -15.00000000000000000 ) ) ;
#11071 = DIRECTION ( 'NONE',  ( -1.000000000000000000, 0.000000000000000000, 0.000000000000000000 ) ) ;
#11072 = CIRCLE ( 'NONE', #17990, 12.49999999999999645 ) ;
#11073 = DIRECTION ( 'NONE',  ( -0.000000000000000000, -0.000000000000000000, 1.000000000000000000 ) ) ;
#11074 = EDGE_CURVE ( 'NONE', #11811, #2802, #18432, .T. ) ;
#11075 = DIRECTION ( 'NONE',  ( 1.000000000000000000, 0.000000000000000000, 0.000000000000000000 ) ) ;
#11076 = EDGE_CURVE ( 'NONE', #5544, #5970, #1954, .T. ) ;
#11077 = CARTESIAN_POINT ( 'NONE',  ( 51.97223112728254790, 46.39948385550240317, 5.992620115222778487 ) ) ;
#11078 = CARTESIAN_POINT ( 'NONE',  ( 0.000000000000000000, 0.5192545390863916310, -1.000000000000000000 ) ) ;
#11079 = CARTESIAN_POINT ( 'NONE',  ( 54.72065718078924590, 60.29948385550240175, 6.458785618021043895 ) ) ;
#11080 = CARTESIAN_POINT ( 'NONE',  ( 54.09612160359792199, 63.30051614449766362, 5.676469297603124353 ) ) ;
#11081 = DIRECTION ( 'NONE',  ( 0.03086419753086420623, -0.9995235871707959241, 0.000000000000000000 ) ) ;
#11082 = VERTEX_POINT ( 'NONE', #6444 ) ;
#11083 = AXIS2_PLACEMENT_3D ( 'NONE', #3932, #5291, #12939 ) ;
#11084 = DIRECTION ( 'NONE',  ( 1.000000000000000000, 0.000000000000000000, 0.000000000000000000 ) ) ;
#11085 = DIRECTION ( 'NONE',  ( 1.000000000000000000, 0.000000000000000000, 0.000000000000000000 ) ) ;
#11086 = CARTESIAN_POINT ( 'NONE',  ( 5.130877905917432535, -39.33065161639846252, -9.000000000000000000 ) ) ;
#11087 = LINE ( 'NONE', #9616, #933 ) ;
#11088 = DIRECTION ( 'NONE',  ( -0.000000000000000000, -0.000000000000000000, -1.000000000000000000 ) ) ;
#11089 = VERTEX_POINT ( 'NONE', #2145 ) ;
#11090 = B_SPLINE_CURVE_WITH_KNOTS ( 'NONE', 3,
 ( #4807, #10770, #16770, #3334, #9296, #11145 ),
 .UNSPECIFIED., .F., .F.,
 ( 4, 2, 4 ),
 ( 0.008261945092156346496, 0.009724140865920691962, 0.01118633663968503569 ),
 .UNSPECIFIED. ) ;
#11091 = DIRECTION ( 'NONE',  ( -0.000000000000000000, 0.000000000000000000, -1.000000000000000000 ) ) ;
#11092 = LINE ( 'NONE', #13849, #2967 ) ;
#11093 = CARTESIAN_POINT ( 'NONE',  ( -54.99999999999996447, -14.99999999999998579, -10.00000000000000000 ) ) ;
#11094 = CARTESIAN_POINT ( 'NONE',  ( 57.36023556966787851, 47.99948385550239038, -0.02388180880522424582 ) ) ;
#11095 = EDGE_CURVE ( 'NONE', #19334, #10178, #8211, .T. ) ;
#11096 = DIRECTION ( 'NONE',  ( 0.000000000000000000, -1.000000000000000000, 0.000000000000000000 ) ) ;
#11097 = CARTESIAN_POINT ( 'NONE',  ( 45.31609314410960820, 60.30051614449767072, -6.485486291978072693 ) ) ;
#11098 = VECTOR ( 'NONE', #5564, 1000.000000000000000 ) ;
#11099 = CARTESIAN_POINT ( 'NONE',  ( 46.45491332379576477, 61.70051614449766220, 4.840751629271188961 ) ) ;
#11100 = EDGE_CURVE ( 'NONE', #5525, #2254, #9478, .T. ) ;
#11101 = CARTESIAN_POINT ( 'NONE',  ( 3.799999999999999378, 0.000000000000000000, -0.8000000000000000444 ) ) ;
#11102 = DIRECTION ( 'NONE',  ( -0.000000000000000000, -0.000000000000000000, 1.000000000000000000 ) ) ;
#11103 = AXIS2_PLACEMENT_3D ( 'NONE', #7170, #17587, #5706 ) ;
#11104 = ORIENTED_EDGE ( 'NONE', *, *, #12318, .F. ) ;
#11105 = EDGE_LOOP ( 'NONE', ( #10912, #4047, #10761, #10271, #12046, #1370, #6387, #15265, #8660, #18108, #16649, #5956, #9065, #18694, #8261, #7339, #1662, #11469, #18940, #6614, #14879, #13271, #9454, #1933, #11256 ) ) ;
#11106 = DIRECTION ( 'NONE',  ( -1.000000000000000000, -4.082155997157843695E-16, 0.000000000000000000 ) ) ;
#11107 = VERTEX_POINT ( 'NONE', #761 ) ;
#11108 = CARTESIAN_POINT ( 'NONE',  ( -4.000000000000000000, 1.941961291383472732, -0.3515519931180205448 ) ) ;
#11109 = VERTEX_POINT ( 'NONE', #10951 ) ;
#11110 = DIRECTION ( 'NONE',  ( 0.000000000000000000, 0.000000000000000000, -1.000000000000000000 ) ) ;
#11111 = CARTESIAN_POINT ( 'NONE',  ( 56.65037692655918988, 51.89948385550241028, -2.184720259617163762 ) ) ;
#11112 = ADVANCED_FACE ( 'NONE', ( #6733 ), #8104, .T. ) ;
#11113 = ORIENTED_EDGE ( 'NONE', *, *, #306, .T. ) ;
#11114 = CARTESIAN_POINT ( 'NONE',  ( -4.078421086530219064, -3.990950201428956845, 0.000000000000000000 ) ) ;
#11115 = ORIENTED_EDGE ( 'NONE', *, *, #18657, .F. ) ;
#11116 = CARTESIAN_POINT ( 'NONE',  ( 52.62207051974839089, 52.39948385550241028, 7.992620115222770494 ) ) ;
#11117 = DIRECTION ( 'NONE',  ( 0.000000000000000000, 0.5150380737757248584, 0.8571673013836862420 ) ) ;
#11118 = CIRCLE ( 'NONE', #1429, 1.000000000000000444 ) ;
#11119 = EDGE_CURVE ( 'NONE', #12796, #2842, #5671, .T. ) ;
#11120 = CARTESIAN_POINT ( 'NONE',  ( 43.69122665457040000, 46.99948385550239749, 0.02388180880521036456 ) ) ;
#11121 = CARTESIAN_POINT ( 'NONE',  ( 4.033901012036116285, 2.321269032827693035, 2.979444097106929146 ) ) ;
#11122 = CARTESIAN_POINT ( 'NONE',  ( 4.175075985190098926, -4.120741555260250877, 2.761631486132788719E-14 ) ) ;
#11123 = CARTESIAN_POINT ( 'NONE',  ( 55.94051828345053679, 59.20051614449766220, 4.345558710429044069 ) ) ;
#11124 = CARTESIAN_POINT ( 'NONE',  ( 49.97728705011488870, 61.49948385550241170, -6.000000000000000888 ) ) ;
#11125 = AXIS2_PLACEMENT_3D ( 'NONE', #14678, #16459, #3130 ) ;
#11126 = CARTESIAN_POINT ( 'NONE',  ( 54.09612160359786515, 57.69948385550240744, -5.676469297603166098 ) ) ;
#11127 = CARTESIAN_POINT ( 'NONE',  ( 6.452281807715817941, -2.898928808472988283, 5.021091983800338276 ) ) ;
#11128 = CARTESIAN_POINT ( 'NONE',  ( 0.000000000000000000, 0.5192545390863916310, 0.000000000000000000 ) ) ;
#11129 = ORIENTED_EDGE ( 'NONE', *, *, #422, .T. ) ;
#11130 = ORIENTED_EDGE ( 'NONE', *, *, #10960, .F. ) ;
#11131 = CARTESIAN_POINT ( 'NONE',  ( 2.000000000000000000, 0.000000000000000000, 0.000000000000000000 ) ) ;
#11132 = CARTESIAN_POINT ( 'NONE',  ( 57.36023556966787851, 53.99948385550239038, -0.02388180880522424582 ) ) ;
#11133 = DIRECTION ( 'NONE',  ( 0.02857142857142857401, -0.9995917534020515305, 0.000000000000000000 ) ) ;
#11134 = ORIENTED_EDGE ( 'NONE', *, *, #4892, .T. ) ;
#11135 = ORIENTED_EDGE ( 'NONE', *, *, #16612, .T. ) ;
#11136 = CARTESIAN_POINT ( 'NONE',  ( 2.449293598294706513E-15, -20.00000000000000000, 9.000000000000000000 ) ) ;
#11137 = AXIS2_PLACEMENT_3D ( 'NONE', #15700, #2279, #11660 ) ;
#11138 = ORIENTED_EDGE ( 'NONE', *, *, #12551, .T. ) ;
#11139 = CARTESIAN_POINT ( 'NONE',  ( -62.49999999999997158, 32.50000000000001421, 15.00000000000000000 ) ) ;
#11140 = VERTEX_POINT ( 'NONE', #567 ) ;
#11141 = CARTESIAN_POINT ( 'NONE',  ( 57.36023556966787851, 45.99948385550238328, -0.02388180880522424582 ) ) ;
#11142 = CARTESIAN_POINT ( 'NONE',  ( -4.999999999999998224, -20.00000000000000000, 15.00000000000000355 ) ) ;
#11143 = CARTESIAN_POINT ( 'NONE',  ( 44.91013252490150620, 62.20051614449766220, -3.727524721679154940 ) ) ;
#11144 = CARTESIAN_POINT ( 'NONE',  ( -154.9999999999999716, -14.99999999999999645, -6.499999999999999112 ) ) ;
#11145 = CARTESIAN_POINT ( 'NONE',  ( 0.4465819873852002742, 2.886751345948125547, 4.999999999999999112 ) ) ;
#11146 = DIRECTION ( 'NONE',  ( 0.000000000000000000, 0.000000000000000000, 1.000000000000000000 ) ) ;
#11147 = CARTESIAN_POINT ( 'NONE',  ( 54.72065718078918906, 60.70051614449766930, -6.458785618021089192 ) ) ;
#11148 = PRODUCT ( 'hex flange bolt small_iso_ISO 4162 - M5 x 40 x 16-N', 'hex flange bolt small_iso_ISO 4162 - M5 x 40 x 16-N', '', ( #14606 ) ) ;
#11149 = ORIENTED_EDGE ( 'NONE', *, *, #16132, .F. ) ;
#11150 = ORIENTED_EDGE ( 'NONE', *, *, #12384, .T. ) ;
#11151 = DIRECTION ( 'NONE',  ( 0.000000000000000000, 0.000000000000000000, -1.000000000000000000 ) ) ;
#11152 = CIRCLE ( 'NONE', #6780, 1.000000000000000000 ) ;
#11153 = CARTESIAN_POINT ( 'NONE',  ( -62.49999999999997158, 32.50000000000001421, 10.00000000000000000 ) ) ;
#11154 = ORIENTED_EDGE ( 'NONE', *, *, #16881, .F. ) ;
#11155 = AXIS2_PLACEMENT_3D ( 'NONE', #16384, #7346, #12769 ) ;
#11156 = CYLINDRICAL_SURFACE ( 'NONE', #6126, 4.000000000000003553 ) ;
#11157 = EDGE_CURVE ( 'NONE', #7151, #5579, #6833, .T. ) ;
#11158 = DIRECTION ( 'NONE',  ( -0.000000000000000000, -0.000000000000000000, 1.000000000000000000 ) ) ;
#11159 = ORIENTED_EDGE ( 'NONE', *, *, #11226, .T. ) ;
#11160 = CIRCLE ( 'NONE', #1798, 1.000000000000000222 ) ;
#11161 = LINE ( 'NONE', #18457, #10024 ) ;
#11162 = DIRECTION ( 'NONE',  ( -1.000000000000000000, 0.000000000000000000, 0.000000000000000000 ) ) ;
#11163 = CYLINDRICAL_SURFACE ( 'NONE', #10461, 1.000000000000000000 ) ;
#11164 = EDGE_CURVE ( 'NONE', #1748, #71, #8805, .T. ) ;
#11165 = LINE ( 'NONE', #18268, #2453 ) ;
#11166 = CARTESIAN_POINT ( 'NONE',  ( 44.05948171654949874, 64.79948385550240175, 4.345558710429105354 ) ) ;
#11167 = CARTESIAN_POINT ( 'NONE',  ( 2.449293598294706513E-15, -20.00000000000000000, -20.00000000000000000 ) ) ;
#11168 = AXIS2_PLACEMENT_3D ( 'NONE', #16702, #17645, #16068 ) ;
#11169 = CARTESIAN_POINT ( 'NONE',  ( 44.05948171654949874, 46.79948385550238754, 4.345558710429105354 ) ) ;
#11170 = CARTESIAN_POINT ( 'NONE',  ( 52.25172492374527877, 61.40051614449765083, 7.007379884777203749 ) ) ;
#11171 = EDGE_CURVE ( 'NONE', #13296, #11691, #15068, .T. ) ;
#11172 = EDGE_CURVE ( 'NONE', #13956, #8949, #2737, .T. ) ;
#11173 = DIRECTION ( 'NONE',  ( 1.000000000000000000, 0.000000000000000000, 0.000000000000000000 ) ) ;
#11174 = CARTESIAN_POINT ( 'NONE',  ( 6.357976367241631621, 3.426708043487392885, -4.282301071214502208 ) ) ;
#11175 = CARTESIAN_POINT ( 'NONE',  ( 2.104978517884645826E-15, -20.00000000000000000, 9.000000000000000000 ) ) ;
#11176 = AXIS2_PLACEMENT_3D ( 'NONE', #13640, #18177, #6196 ) ;
#11177 = ORIENTED_EDGE ( 'NONE', *, *, #8208, .F. ) ;
#11178 = FACE_OUTER_BOUND ( 'NONE', #6590, .T. ) ;
#11179 = ADVANCED_FACE ( 'NONE', ( #5757 ), #19218, .F. ) ;
#11180 = EDGE_CURVE ( 'NONE', #2296, #18086, #10368, .T. ) ;
#11181 = CARTESIAN_POINT ( 'NONE',  ( 13.99999999999999822, 0.000000000000000000, 1.610000000000000098 ) ) ;
#11182 = VECTOR ( 'NONE', #7522, 1000.000000000000000 ) ;
#11183 = CARTESIAN_POINT ( 'NONE',  ( 43.34962307344078880, 50.10051614449766078, -2.184720259617096705 ) ) ;
#11184 = CARTESIAN_POINT ( 'NONE',  ( -14.86289650954781649, -33.38261212717723936, 9.000000000000000000 ) ) ;
#11185 = CYLINDRICAL_SURFACE ( 'NONE', #9300, 3.799999999999993605 ) ;
#11186 = VERTEX_POINT ( 'NONE', #8793 ) ;
#11187 = CARTESIAN_POINT ( 'NONE',  ( -179.9999999999999716, -14.99999999999999289, 3.999999999999999112 ) ) ;
#11188 = DIRECTION ( 'NONE',  ( 0.000000000000000000, 0.000000000000000000, -1.000000000000000000 ) ) ;
#11189 = EDGE_CURVE ( 'NONE', #12590, #13221, #8545, .T. ) ;
#11190 = CYLINDRICAL_SURFACE ( 'NONE', #7141, 4.000000000000003553 ) ;
#11191 = CARTESIAN_POINT ( 'NONE',  ( 5.100000000000002309, 6.368163355566238354E-16, -5.200000000000001066 ) ) ;
#11192 = EDGE_CURVE ( 'NONE', #6090, #10132, #6929, .T. ) ;
#11193 = CARTESIAN_POINT ( 'NONE',  ( -54.99999999999996447, -22.99999999999998579, -10.00000000000000000 ) ) ;
#11194 = CIRCLE ( 'NONE', #17167, 1.000000000000000222 ) ;
#11195 = CARTESIAN_POINT ( 'NONE',  ( 52.62207051974829852, 60.60051614449765367, -7.992620115222797139 ) ) ;
#11196 = CARTESIAN_POINT ( 'NONE',  ( 46.49166364869456913, 62.30051614449766362, -4.867452303228181343 ) ) ;
#11197 = VECTOR ( 'NONE', #8539, 1000.000000000000000 ) ;
#11198 = ADVANCED_FACE ( 'NONE', ( #15862 ), #9729, .T. ) ;
#11199 = CARTESIAN_POINT ( 'NONE',  ( 2.449293598294706513E-15, -20.00000000000000000, -20.00000000000000000 ) ) ;
#11200 = CARTESIAN_POINT ( 'NONE',  ( 4.898587196589413026E-15, -40.00000000000000000, 9.000000000000000000 ) ) ;
#11201 = ORIENTED_EDGE ( 'NONE', *, *, #710, .F. ) ;
#11202 = ORIENTED_EDGE ( 'NONE', *, *, #16843, .T. ) ;
#11203 =( GEOMETRIC_REPRESENTATION_CONTEXT ( 3 ) GLOBAL_UNCERTAINTY_ASSIGNED_CONTEXT ( ( #14794 ) ) GLOBAL_UNIT_ASSIGNED_CONTEXT ( ( #11448, #9974, #7243 ) ) REPRESENTATION_CONTEXT ( 'NONE', 'WORKASPACE' ) );
#11204 = ORIENTED_EDGE ( 'NONE', *, *, #12280, .F. ) ;
#11205 = CARTESIAN_POINT ( 'NONE',  ( 1.567478505476134606E-15, 4.618802153517012066, -5.000000000000000000 ) ) ;
#11206 = ORIENTED_EDGE ( 'NONE', *, *, #12790, .F. ) ;
#11207 = DIRECTION ( 'NONE',  ( -1.000000000000000000, 0.000000000000000000, 0.000000000000000000 ) ) ;
#11208 = EDGE_LOOP ( 'NONE', ( #5481, #8714, #12110, #689 ) ) ;
#11209 = DIRECTION ( 'NONE',  ( 1.000000000000000000, 0.000000000000000000, 0.000000000000000000 ) ) ;
#11210 = MECHANICAL_DESIGN_GEOMETRIC_PRESENTATION_REPRESENTATION (  '', ( #1840 ), #5897 ) ;
#11211 = CARTESIAN_POINT ( 'NONE',  ( 44.03140696652193498, 59.19948385550240033, -4.306917132069424170 ) ) ;
#11212 = EDGE_LOOP ( 'NONE', ( #11603, #15094, #17480, #19252 ) ) ;
#11213 = CARTESIAN_POINT ( 'NONE',  ( 6.385552186430389021, -2.886751345948133984, -5.000000000000000000 ) ) ;
#11214 = ORIENTED_EDGE ( 'NONE', *, *, #5708, .T. ) ;
#11215 = CARTESIAN_POINT ( 'NONE',  ( 57.61547081786812896, 50.09948385550240602, 2.450534656007040901 ) ) ;
#11216 = CARTESIAN_POINT ( 'NONE',  ( 3.961545574370306966, 1.423222908132971476, -3.499999999999999556 ) ) ;
#11217 = CARTESIAN_POINT ( 'NONE',  ( 47.70284917648453415, 63.39948385550240317, -6.992620115222774047 ) ) ;
#11218 = CARTESIAN_POINT ( 'NONE',  ( 4.086262629614028086, 1.979770830881088850, 3.570936333571100629 ) ) ;
#11219 = LINE ( 'NONE', #17225, #17473 ) ;
#11220 = CARTESIAN_POINT ( 'NONE',  ( 52.25172492374527877, 61.40051614449765083, 7.007379884777203749 ) ) ;
#11221 = CARTESIAN_POINT ( 'NONE',  ( 46.45491332379576477, 45.70051614449766220, 4.840751629271188961 ) ) ;
#11222 = CARTESIAN_POINT ( 'NONE',  ( 45.90387839640214196, 56.69948385550240744, 5.676469297603166098 ) ) ;
#11223 = CARTESIAN_POINT ( 'NONE',  ( 6.534224484704323821, -2.950930484791555841, 5.111161529262928660 ) ) ;
#11224 = CARTESIAN_POINT ( 'NONE',  ( 49.99999999999997158, 45.00000000000001421, -6.500000000000004441 ) ) ;
#11225 = EDGE_LOOP ( 'NONE', ( #9399, #16642, #2457, #10506 ) ) ;
#11226 = EDGE_CURVE ( 'NONE', #14655, #15873, #4097, .T. ) ;
#11227 = ORIENTED_EDGE ( 'NONE', *, *, #2137, .F. ) ;
#11228 = CARTESIAN_POINT ( 'NONE',  ( 0.000000000000000000, 0.000000000000000000, 9.999999999999998224 ) ) ;
#11229 = VERTEX_POINT ( 'NONE', #10066 ) ;
#11230 = ADVANCED_FACE ( 'NONE', ( #7130 ), #11632, .F. ) ;
#11231 = CARTESIAN_POINT ( 'NONE',  ( 44.03140696652192787, 61.19948385550239323, -4.306917132069425058 ) ) ;
#11232 = CYLINDRICAL_SURFACE ( 'NONE', #5925, 4.799999999999999822 ) ;
#11233 =( GEOMETRIC_REPRESENTATION_CONTEXT ( 3 ) GLOBAL_UNCERTAINTY_ASSIGNED_CONTEXT ( ( #288 ) ) GLOBAL_UNIT_ASSIGNED_CONTEXT ( ( #7865, #6774, #8146 ) ) REPRESENTATION_CONTEXT ( 'NONE', 'WORKASPACE' ) );
#11234 = ORIENTED_EDGE ( 'NONE', *, *, #3385, .T. ) ;
#11235 = VERTEX_POINT ( 'NONE', #1347 ) ;
#11236 = DIRECTION ( 'NONE',  ( 0.000000000000000000, 0.000000000000000000, -1.000000000000000000 ) ) ;
#11237 = ORIENTED_EDGE ( 'NONE', *, *, #2928, .T. ) ;
#11238 = DIRECTION ( 'NONE',  ( 0.3420201433256622736, 1.150791560227853228E-16, 0.9396926207859106484 ) ) ;
#11239 = ORIENTED_EDGE ( 'NONE', *, *, #11901, .F. ) ;
#11240 = CIRCLE ( 'NONE', #6860, 5.000000000000007994 ) ;
#11241 = AXIS2_PLACEMENT_3D ( 'NONE', #18596, #3670, #11398 ) ;
#11242 = CARTESIAN_POINT ( 'NONE',  ( 56.66441430157296821, 48.09948385550240602, 2.141517661632100111 ) ) ;
#11243 = DIRECTION ( 'NONE',  ( -1.000000000000000000, 0.000000000000000000, 0.000000000000000000 ) ) ;
#11244 = CARTESIAN_POINT ( 'NONE',  ( 51.92680522751238925, 59.40051614449765793, 6.007379884777208190 ) ) ;
#11245 = FACE_OUTER_BOUND ( 'NONE', #16150, .T. ) ;
#11246 = APPLICATION_CONTEXT ( 'automotive_design' ) ;
#11247 = DIRECTION ( 'NONE',  ( 0.000000000000000000, -0.4999999999999989453, 0.8660254037844391517 ) ) ;
#11248 = AXIS2_PLACEMENT_3D ( 'NONE', #5803, #11765, #16304 ) ;
#11249 = DIRECTION ( 'NONE',  ( 0.000000000000000000, 0.000000000000000000, 1.000000000000000000 ) ) ;
#11250 = ORIENTED_EDGE ( 'NONE', *, *, #13223, .T. ) ;
#11251 = VERTEX_POINT ( 'NONE', #2549 ) ;
#11252 = CARTESIAN_POINT ( 'NONE',  ( 4.000000000000000000, -0.8732470631449981147, -3.223155494240760088 ) ) ;
#11253 = CIRCLE ( 'NONE', #7502, 3.500000000000000000 ) ;
#11254 =( LENGTH_UNIT ( ) NAMED_UNIT ( * ) SI_UNIT ( .MILLI., .METRE. ) );
#11255 = ITEM_DEFINED_TRANSFORMATION ( 'NONE', 'NONE', #6549,  #10359 ) ;
#11256 = ORIENTED_EDGE ( 'NONE', *, *, #8957, .T. ) ;
#11257 = DIRECTION ( 'NONE',  ( -1.000000000000000000, 0.000000000000000000, 0.000000000000000000 ) ) ;
#11258 = DIRECTION ( 'NONE',  ( -0.9768494444668813781, -0.2139279384389642935, 1.428280402115105433E-22 ) ) ;
#11259 = AXIS2_PLACEMENT_3D ( 'NONE', #4765, #16724, #3285 ) ;
#11260 = VERTEX_POINT ( 'NONE', #19116 ) ;
#11261 = CARTESIAN_POINT ( 'NONE',  ( -154.8505191518487152, -18.79705879280739467, -15.79999999999999893 ) ) ;
#11262 = CARTESIAN_POINT ( 'NONE',  ( -54.99999999999996447, -14.99999999999998579, -10.00000000000000178 ) ) ;
#11263 = CARTESIAN_POINT ( 'NONE',  ( 3.333333333333335702, -2.694301256218268215, -3.300726591567084256 ) ) ;
#11264 = DIRECTION ( 'NONE',  ( -1.000000000000000000, 0.000000000000000000, 0.000000000000000000 ) ) ;
#11265 = CARTESIAN_POINT ( 'NONE',  ( 50.02271294988511841, 48.49948385550241170, 6.000000000000000888 ) ) ;
#11266 = CIRCLE ( 'NONE', #15356, 3.500000000000000000 ) ;
#11267 = CARTESIAN_POINT ( 'NONE',  ( -1.250000000000000000, -6.429618962271402616, -1.000000000000000000 ) ) ;
#11268 = AXIS2_PLACEMENT_3D ( 'NONE', #1730, #2920, #13495 ) ;
#11269 = CARTESIAN_POINT ( 'NONE',  ( 56.66441430157296821, 48.09948385550240602, 2.141517661632100111 ) ) ;
#11270 = ADVANCED_FACE ( 'NONE', ( #18919 ), #16064, .F. ) ;
#11271 = CARTESIAN_POINT ( 'NONE',  ( 50.02271294988505446, 60.50051614449765935, -7.000000000000000888 ) ) ;
#11272 = VECTOR ( 'NONE', #13260, 1000.000000000000000 ) ;
#11273 = DIRECTION ( 'NONE',  ( -1.000000000000000000, -0.000000000000000000, -0.000000000000000000 ) ) ;
#11274 = DIRECTION ( 'NONE',  ( 0.000000000000000000, 0.000000000000000000, 1.000000000000000000 ) ) ;
#11275 = CARTESIAN_POINT ( 'NONE',  ( -62.49999999999997158, 32.50000000000001421, 20.60000000000000142 ) ) ;
#11276 =( REPRESENTATION_RELATIONSHIP ('NONE','NONE', #16703, #1926 ) REPRESENTATION_RELATIONSHIP_WITH_TRANSFORMATION ( #18358 )SHAPE_REPRESENTATION_RELATIONSHIP( ) );
#11277 = VERTEX_POINT ( 'NONE', #7322 ) ;
#11278 = CIRCLE ( 'NONE', #5036, 1.000000000000000222 ) ;
#11279 = CARTESIAN_POINT ( 'NONE',  ( -17.32050807568879236, -10.00000000000004263, 9.000000000000000000 ) ) ;
#11280 = DIRECTION ( 'NONE',  ( -0.7071067811865350272, 0.000000000000000000, 0.7071067811865598962 ) ) ;
#11281 = AXIS2_PLACEMENT_3D ( 'NONE', #2630, #12805, #1047 ) ;
#11282 = AXIS2_PLACEMENT_3D ( 'NONE', #4352, #14738, #17993 ) ;
#11283 = CARTESIAN_POINT ( 'NONE',  ( 49.97728705011495265, 53.50051614449765935, 7.000000000000000888 ) ) ;
#11284 = CARTESIAN_POINT ( 'NONE',  ( 52.07576163693497051, 45.00000000000001421, -7.275735003127095979 ) ) ;
#11285 = EDGE_CURVE ( 'NONE', #9040, #7722, #5460, .T. ) ;
#11286 = PRESENTATION_LAYER_ASSIGNMENT (  '', '', ( #1921 ) ) ;
#11287 = CARTESIAN_POINT ( 'NONE',  ( 2.449293598294706513E-15, -20.00000000000000000, 9.000000000000000000 ) ) ;
#11288 = ORIENTED_EDGE ( 'NONE', *, *, #5329, .F. ) ;
#11289 = CARTESIAN_POINT ( 'NONE',  ( -1.250000000000000000, -6.429618962271402616, -1.000000000000000000 ) ) ;
#11290 = CARTESIAN_POINT ( 'NONE',  ( 0.3126073911696451990, -4.041451884327386779, -1.834154111220703958E-17 ) ) ;
#11291 = CARTESIAN_POINT ( 'NONE',  ( -54.99999999999996447, -6.999999999999985789, 10.00000000000000000 ) ) ;
#11292 = CARTESIAN_POINT ( 'NONE',  ( 44.05948171654949874, 48.79948385550238754, 4.345558710429105354 ) ) ;
#11293 =( BOUNDED_SURFACE ( )  B_SPLINE_SURFACE ( 3, 2, ( 
 ( #7647, #8923, #3059 ),
 ( #110, #3154, #15106 ),
 ( #7456, #2960, #7360 ),
 ( #4526, #13437, #9120 ),
 ( #8831, #6089, #1683 ),
 ( #1384, #6001, #18059 ) ),
 .UNSPECIFIED., .F., .F., .F. ) 
 B_SPLINE_SURFACE_WITH_KNOTS ( ( 4, 2, 4 ),
 ( 3, 3 ),
 ( 0.01651999345535503164, 0.01858032176739832925, 0.02064065007944162339 ),
 ( 0.000000000000000000, 1.000000000000000000 ),
 .UNSPECIFIED. ) 
 GEOMETRIC_REPRESENTATION_ITEM ( )  RATIONAL_B_SPLINE_SURFACE ( (
 ( 1.000000000000000000, 0.8047781103519391355, 1.000000000000000000),
 ( 1.000000000000000000, 0.8123785825612301892, 1.000000000000000000),
 ( 1.000000000000000000, 0.8190671539777686361, 1.000000000000000000),
 ( 1.000000000000000000, 0.8192352254845479687, 1.000000000000000000),
 ( 1.000000000000000000, 0.8126129677203643986, 1.000000000000000000),
 ( 1.000000000000000000, 0.8047712537969725632, 1.000000000000000000) ) ) 
 REPRESENTATION_ITEM ( '' )  SURFACE ( )  );
#11294 = CARTESIAN_POINT ( 'NONE',  ( -2.345747346278108214, 3.264484291692489215, -0.01223254789873409049 ) ) ;
#11295 = CARTESIAN_POINT ( 'NONE',  ( 42.39856655714566358, 48.89948385550241028, 2.493737253992119207 ) ) ;
#11296 = DIRECTION ( 'NONE',  ( -0.000000000000000000, -0.000000000000000000, 1.000000000000000000 ) ) ;
#11297 = EDGE_CURVE ( 'NONE', #8220, #5480, #1059, .T. ) ;
#11298 = CARTESIAN_POINT ( 'NONE',  ( 44.28664221472221385, 59.90051614449767214, 1.832500667257213722 ) ) ;
#11299 = EDGE_CURVE ( 'NONE', #9833, #6603, #13107, .T. ) ;
#11300 = DIRECTION ( 'NONE',  ( 0.000000000000000000, -0.000000000000000000, 1.000000000000000000 ) ) ;
#11301 = AXIS2_PLACEMENT_3D ( 'NONE', #10852, #16861, #3420 ) ;
#11302 = CARTESIAN_POINT ( 'NONE',  ( 3.973110223765528914, 0.6902454861566579281, -3.565797985667391146 ) ) ;
#11303 = EDGE_LOOP ( 'NONE', ( #4095, #13292, #11134, #5705 ) ) ;
#11304 = EDGE_CURVE ( 'NONE', #2993, #12017, #6601, .T. ) ;
#11305 = ORIENTED_EDGE ( 'NONE', *, *, #10638, .F. ) ;
#11306 = ORIENTED_EDGE ( 'NONE', *, *, #17333, .T. ) ;
#11307 = CARTESIAN_POINT ( 'NONE',  ( -0.1085714285714285687, -3.798448662927795372, -0.8000000000000000444 ) ) ;
#11308 = EDGE_LOOP ( 'NONE', ( #10220, #4412 ) ) ;
#11309 = EDGE_CURVE ( 'NONE', #3228, #9645, #989, .T. ) ;
#11310 = CARTESIAN_POINT ( 'NONE',  ( 3.974183935050568106, -0.7239581970520293508, 3.565826011443134824 ) ) ;
#11311 = ORIENTED_EDGE ( 'NONE', *, *, #644, .F. ) ;
#11312 = DIRECTION ( 'NONE',  ( -1.000000000000000000, 0.000000000000000000, 0.000000000000000000 ) ) ;
#11313 = CARTESIAN_POINT ( 'NONE',  ( 57.36023556966787851, 57.99948385550240459, -0.02388180880522424582 ) ) ;
#11314 = EDGE_LOOP ( 'NONE', ( #10175, #5644 ) ) ;
#11315 = LINE ( 'NONE', #7095, #14931 ) ;
#11316 = ORIENTED_EDGE ( 'NONE', *, *, #417, .F. ) ;
#11317 = CARTESIAN_POINT ( 'NONE',  ( 56.79116909180255135, 51.79948385550240175, -4.963592699179005585 ) ) ;
#11318 = CARTESIAN_POINT ( 'NONE',  ( 2.345747346278113987, -3.264484291692503870, -0.01223254789874484924 ) ) ;
#11319 = PRODUCT_DEFINITION_SHAPE ( 'NONE', 'NONE',  #19422 ) ;
#11320 = CARTESIAN_POINT ( 'NONE',  ( 44.91013252490152752, 48.79948385550240175, 3.727524721679198461 ) ) ;
#11321 = CARTESIAN_POINT ( 'NONE',  ( 4.180231891692618440, 2.049421325483208101, 3.591231015387272851 ) ) ;
#11322 = COLOUR_RGB ( '',1.000000000000000000, 0.9490196078431372140, 0.9098039215686274384 ) ;
#11323 = DIRECTION ( 'NONE',  ( -0.000000000000000000, -0.000000000000000000, -1.000000000000000000 ) ) ;
#11324 = CARTESIAN_POINT ( 'NONE',  ( 43.18075615816994173, 47.80051614449764941, 4.924951120819380357 ) ) ;
#11325 = ADVANCED_FACE ( 'NONE', ( #11920 ), #10538, .F. ) ;
#11326 = CARTESIAN_POINT ( 'NONE',  ( 51.92680522751238925, 45.40051614449765793, 6.007379884777208190 ) ) ;
#11327 = EDGE_CURVE ( 'NONE', #3087, #8364, #18120, .T. ) ;
#11328 = CARTESIAN_POINT ( 'NONE',  ( -1.250000000000001110, 7.286648454926751965E-16, 5.899999999999999467 ) ) ;
#11329 = DIRECTION ( 'NONE',  ( 0.000000000000000000, -0.000000000000000000, 1.000000000000000000 ) ) ;
#11330 = ORIENTED_EDGE ( 'NONE', *, *, #2876, .F. ) ;
#11331 = ORIENTED_EDGE ( 'NONE', *, *, #9176, .T. ) ;
#11332 = DIRECTION ( 'NONE',  ( -1.000000000000000000, 0.000000000000000000, -0.000000000000000000 ) ) ;
#11333 = ORIENTED_EDGE ( 'NONE', *, *, #14293, .F. ) ;
#11334 = CARTESIAN_POINT ( 'NONE',  ( 54.13287192849676188, 58.29948385550240175, 5.649768623646098220 ) ) ;
#11335 = PLANE ( 'NONE',  #19407 ) ;
#11336 = ORIENTED_EDGE ( 'NONE', *, *, #7882, .T. ) ;
#11337 = ORIENTED_EDGE ( 'NONE', *, *, #18145, .T. ) ;
#11338 = DIRECTION ( 'NONE',  ( 0.000000000000000000, 0.000000000000000000, 1.000000000000000000 ) ) ;
#11339 = VERTEX_POINT ( 'NONE', #3119 ) ;
#11340 = CARTESIAN_POINT ( 'NONE',  ( 2.000000000000000000, 0.000000000000000000, 0.000000000000000000 ) ) ;
#11341 = ORIENTED_EDGE ( 'NONE', *, *, #118, .T. ) ;
#11342 = CARTESIAN_POINT ( 'NONE',  ( 43.34962307344081012, 52.89948385550240317, 2.184720259617164650 ) ) ;
#11343 = DIRECTION ( 'NONE',  ( 0.000000000000000000, 0.000000000000000000, -1.000000000000000000 ) ) ;
#11344 = CIRCLE ( 'NONE', #2913, 12.49999999999999645 ) ;
#11345 = CARTESIAN_POINT ( 'NONE',  ( 50.02271294988506156, 62.50051614449767357, -6.000000000000000888 ) ) ;
#11346 = FACE_OUTER_BOUND ( 'NONE', #10037, .T. ) ;
#11347 = EDGE_CURVE ( 'NONE', #258, #11140, #6306, .T. ) ;
#11348 = DIRECTION ( 'NONE',  ( 1.000000000000000000, 0.000000000000000000, 0.000000000000000000 ) ) ;
#11349 = EDGE_CURVE ( 'NONE', #15181, #18044, #12564, .T. ) ;
#11350 = DIRECTION ( 'NONE',  ( 0.000000000000000000, 0.000000000000000000, 1.000000000000000000 ) ) ;
#11351 = EDGE_CURVE ( 'NONE', #5162, #16099, #13588, .T. ) ;
#11352 = EDGE_LOOP ( 'NONE', ( #6956, #3865, #9356 ) ) ;
#11353 = ORIENTED_EDGE ( 'NONE', *, *, #7489, .T. ) ;
#11354 = CARTESIAN_POINT ( 'NONE',  ( 4.211405965630455661, 2.460463115436283932, -3.751298928144577882 ) ) ;
#11355 = DIRECTION ( 'NONE',  ( 0.000000000000000000, 0.000000000000000000, -1.000000000000000000 ) ) ;
#11356 = DIRECTION ( 'NONE',  ( -0.000000000000000000, -0.000000000000000000, 1.000000000000000000 ) ) ;
#11357 = ORIENTED_EDGE ( 'NONE', *, *, #1914, .T. ) ;
#11358 = CARTESIAN_POINT ( 'NONE',  ( 6.245824673232988289, 3.903127342724162840, 3.450227696316072734 ) ) ;
#11359 = ORIENTED_EDGE ( 'NONE', *, *, #2156, .T. ) ;
#11360 = ADVANCED_FACE ( 'NONE', ( #6053 ), #17274, .T. ) ;
#11361 = CARTESIAN_POINT ( 'NONE',  ( 54.23491683972284960, 45.00000000000001421, -4.999999999999999112 ) ) ;
#11362 = DIRECTION ( 'NONE',  ( -1.000000000000000000, 0.000000000000000000, -0.000000000000000000 ) ) ;
#11363 = CARTESIAN_POINT ( 'NONE',  ( 46.45491332379572924, 61.29948385550240886, -4.840751629271157874 ) ) ;
#11364 = LINE ( 'NONE', #17468, #2669 ) ;
#11365 = EDGE_CURVE ( 'NONE', #2561, #14864, #13679, .T. ) ;
#11366 = DIRECTION ( 'NONE',  ( -1.000000000000000000, -0.000000000000000000, -0.000000000000000000 ) ) ;
#11367 = CARTESIAN_POINT ( 'NONE',  ( 46.45491332379572924, 51.29948385550240175, -4.840751629271157874 ) ) ;
#11368 = DIRECTION ( 'NONE',  ( 0.000000000000000000, 0.000000000000000000, 1.000000000000000000 ) ) ;
#11369 = CARTESIAN_POINT ( 'NONE',  ( 49.97728705011488159, 47.49948385550240459, -7.000000000000000888 ) ) ;
#11370 = CARTESIAN_POINT ( 'NONE',  ( 50.02271294988505446, 50.50051614449765935, -8.000000000000001776 ) ) ;
#11371 = CARTESIAN_POINT ( 'NONE',  ( -54.99999999999996447, -22.99999999999998579, 15.00000000000000000 ) ) ;
#11372 = CARTESIAN_POINT ( 'NONE',  ( 3.309651814758565180, -5.455921364805393026, -1.000000000000000000 ) ) ;
#11373 = DIRECTION ( 'NONE',  ( 0.9237280213470682178, 0.3830490080632377725, 0.000000000000000000 ) ) ;
#11374 = ORIENTED_EDGE ( 'NONE', *, *, #5802, .T. ) ;
#11375 = PRESENTATION_STYLE_ASSIGNMENT (( #17090 ) ) ;
#11376 = VECTOR ( 'NONE', #16714, 1000.000000000000000 ) ;
#11377 = DIRECTION ( 'NONE',  ( 0.000000000000000000, 0.000000000000000000, 1.000000000000000000 ) ) ;
#11378 = CARTESIAN_POINT ( 'NONE',  ( 45.86712807150329496, 55.70051614449766220, 5.649768623646139964 ) ) ;
#11379 = CIRCLE ( 'NONE', #11705, 8.000000000000007105 ) ;
#11380 = CARTESIAN_POINT ( 'NONE',  ( -4.211140560182196957, 2.431303136016537803, -3.745885042887433514 ) ) ;
#11381 = DIRECTION ( 'NONE',  ( 1.000000000000000000, 0.000000000000000000, 0.000000000000000000 ) ) ;
#11382 = ORIENTED_EDGE ( 'NONE', *, *, #2943, .T. ) ;
#11383 = CARTESIAN_POINT ( 'NONE',  ( 32.00000000000000000, 3.000000000000000000, 6.000000000000000000 ) ) ;
#11384 = DIRECTION ( 'NONE',  ( 1.000000000000000000, 0.000000000000000000, 0.000000000000000000 ) ) ;
#11385 = DIRECTION ( 'NONE',  ( 1.000000000000000000, 0.000000000000000000, 0.000000000000000000 ) ) ;
#11386 = CARTESIAN_POINT ( 'NONE',  ( 44.05948171654949874, 50.79948385550238754, 4.345558710429105354 ) ) ;
#11387 = CYLINDRICAL_SURFACE ( 'NONE', #12953, 0.5999999999999998668 ) ;
#11388 = CARTESIAN_POINT ( 'NONE',  ( 43.18075615816989199, 47.19948385550240744, -4.924951120819313743 ) ) ;
#11389 =( NAMED_UNIT ( * ) SI_UNIT ( $, .STERADIAN. ) SOLID_ANGLE_UNIT ( ) );
#11390 = CARTESIAN_POINT ( 'NONE',  ( 54.09612160359792199, 45.30051614449766362, 5.676469297603124353 ) ) ;
#11391 = CIRCLE ( 'NONE', #2021, 24.99999999999999289 ) ;
#11392 = CARTESIAN_POINT ( 'NONE',  ( 14.00000000000000000, 15.00000000000001776, -9.000000000000000000 ) ) ;
#11393 = APPLICATION_CONTEXT ( 'automotive_design' ) ;
#11394 = CARTESIAN_POINT ( 'NONE',  ( -15.51323935927273645, -7.377028694403556131, 9.000000000000000000 ) ) ;
#11395 = AXIS2_PLACEMENT_3D ( 'NONE', #13912, #9504, #14009 ) ;
#11396 = EDGE_LOOP ( 'NONE', ( #2273, #7983 ) ) ;
#11397 = ORIENTED_EDGE ( 'NONE', *, *, #7357, .F. ) ;
#11398 = DIRECTION ( 'NONE',  ( 1.000000000000000000, 0.000000000000000000, 0.000000000000000000 ) ) ;
#11399 = ORIENTED_EDGE ( 'NONE', *, *, #17483, .F. ) ;
#11400 = CARTESIAN_POINT ( 'NONE',  ( 4.086262418390198548, -2.102635014057361751, 3.500000000000000444 ) ) ;
#11401 = ORIENTED_EDGE ( 'NONE', *, *, #2996, .F. ) ;
#11402 = DIRECTION ( 'NONE',  ( 0.000000000000000000, 0.000000000000000000, -1.000000000000000000 ) ) ;
#11403 = EDGE_CURVE ( 'NONE', #273, #9070, #4438, .T. ) ;
#11404 = CARTESIAN_POINT ( 'NONE',  ( 47.74827507625477807, 56.59948385550240602, 7.007379884777229506 ) ) ;
#11405 = VERTEX_POINT ( 'NONE', #10641 ) ;
#11406 = CARTESIAN_POINT ( 'NONE',  ( -154.8426517387881347, -18.99690399242885874, 17.00000000000000000 ) ) ;
#11407 = ORIENTED_EDGE ( 'NONE', *, *, #12800, .F. ) ;
#11408 =( BOUNDED_SURFACE ( )  B_SPLINE_SURFACE ( 3, 2, ( 
 ( #15327, #1906, #2495 ),
 ( #8452, #8346, #9814 ),
 ( #19238, #3951, #9911 ),
 ( #4415, #15813, #4 ),
 ( #14432, #3045, #14326 ),
 ( #14992, #5315, #908 ) ),
 .UNSPECIFIED., .F., .F., .F. ) 
 B_SPLINE_SURFACE_WITH_KNOTS ( ( 4, 2, 4 ),
 ( 3, 3 ),
 ( 0.01651999345535504551, 0.01858032176739835006, 0.02064065007944165114 ),
 ( 0.000000000000000000, 1.000000000000000000 ),
 .UNSPECIFIED. ) 
 GEOMETRIC_REPRESENTATION_ITEM ( )  RATIONAL_B_SPLINE_SURFACE ( (
 ( 1.000000000000000000, 0.8047781103519391355, 1.000000000000000000),
 ( 1.000000000000000000, 0.8123785825613523137, 1.000000000000000000),
 ( 1.000000000000000000, 0.8190671539776074317, 1.000000000000000000),
 ( 1.000000000000000000, 0.8192352254847047321, 1.000000000000000000),
 ( 1.000000000000000000, 0.8126129677202470480, 1.000000000000000000),
 ( 1.000000000000000000, 0.8047712537969722302, 1.000000000000000000) ) ) 
 REPRESENTATION_ITEM ( '' )  SURFACE ( )  );
#11409 = CARTESIAN_POINT ( 'NONE',  ( 52.57664461997811856, 57.59948385550240602, -8.007379884777229506 ) ) ;
#11410 = AXIS2_PLACEMENT_3D ( 'NONE', #10383, #13231, #11748 ) ;
#11411 = CARTESIAN_POINT ( 'NONE',  ( 0.1388410611046073107, 2.351840044243033834, -2.926493552096022022 ) ) ;
#11412 = EDGE_CURVE ( 'NONE', #11822, #4387, #6237, .T. ) ;
#11413 = CARTESIAN_POINT ( 'NONE',  ( 50.02271294988511841, 50.49948385550239749, 6.000000000000000888 ) ) ;
#11414 = CARTESIAN_POINT ( 'NONE',  ( -158.9999999999999716, -14.99999999999999645, -6.499999999999999112 ) ) ;
#11415 = FACE_OUTER_BOUND ( 'NONE', #7744, .T. ) ;
#11416 = CARTESIAN_POINT ( 'NONE',  ( 43.20883090819742023, 48.20051614449766930, -4.963592699178938972 ) ) ;
#11417 = AXIS2_PLACEMENT_3D ( 'NONE', #19060, #18959, #1005 ) ;
#11418 = EDGE_CURVE ( 'NONE', #11339, #3030, #1648, .T. ) ;
#11419 = CARTESIAN_POINT ( 'NONE',  ( 53.50833635130540955, 63.69948385550240033, -4.867452303228209765 ) ) ;
#11420 = ADVANCED_FACE ( 'NONE', ( #2923 ), #1542, .T. ) ;
#11421 = CARTESIAN_POINT ( 'NONE',  ( 20.00000000000000000, -25.00000000000000711, -20.00000000000000000 ) ) ;
#11422 = PLANE ( 'NONE',  #9387 ) ;
#11423 = VERTEX_POINT ( 'NONE', #10352 ) ;
#11424 = ADVANCED_FACE ( 'NONE', ( #12210 ), #18020, .T. ) ;
#11425 = ORIENTED_EDGE ( 'NONE', *, *, #7696, .T. ) ;
#11426 = CARTESIAN_POINT ( 'NONE',  ( 0.000000000000000000, 0.8865213383406680414, -1.535500000000000975 ) ) ;
#11427 = ORIENTED_EDGE ( 'NONE', *, *, #5122, .T. ) ;
#11428 = CARTESIAN_POINT ( 'NONE',  ( 50.02271294988512551, 60.49948385550240459, 7.000000000000000888 ) ) ;
#11429 = DIRECTION ( 'NONE',  ( 1.000000000000000000, 0.000000000000000000, 0.000000000000000000 ) ) ;
#11430 = ORIENTED_EDGE ( 'NONE', *, *, #6332, .T. ) ;
#11431 = ORIENTED_EDGE ( 'NONE', *, *, #16591, .T. ) ;
#11432 = CARTESIAN_POINT ( 'NONE',  ( -14.86289650954781649, -33.38261212717723936, -9.000000000000000000 ) ) ;
#11433 = AXIS2_PLACEMENT_3D ( 'NONE', #210, #10780, #12160 ) ;
#11434 = EDGE_CURVE ( 'NONE', #6154, #13316, #16647, .T. ) ;
#11435 = ADVANCED_FACE ( 'NONE', ( #8979 ), #9117, .T. ) ;
#11436 = EDGE_LOOP ( 'NONE', ( #11517, #1622, #6730, #8785 ) ) ;
#11437 = CARTESIAN_POINT ( 'NONE',  ( -1.149999999999998135, 0.000000000000000000, 0.000000000000000000 ) ) ;
#11438 = ORIENTED_EDGE ( 'NONE', *, *, #8565, .F. ) ;
#11439 = CARTESIAN_POINT ( 'NONE',  ( 54.09612160359786515, 49.69948385550240744, -5.676469297603166098 ) ) ;
#11440 = DIRECTION ( 'NONE',  ( -0.000000000000000000, -0.000000000000000000, 1.000000000000000000 ) ) ;
#11441 = CARTESIAN_POINT ( 'NONE',  ( 47.74827507625469281, 46.40051614449764372, -7.007379884777203749 ) ) ;
#11442 = DIRECTION ( 'NONE',  ( -1.000000000000000000, 0.000000000000000000, 0.000000000000000000 ) ) ;
#11443 = LINE ( 'NONE', #14285, #8150 ) ;
#11444 = CIRCLE ( 'NONE', #6137, 3.500000000000000000 ) ;
#11445 = EDGE_LOOP ( 'NONE', ( #18262, #8227, #1589, #6821 ) ) ;
#11446 = ORIENTED_EDGE ( 'NONE', *, *, #13760, .T. ) ;
#11447 = CARTESIAN_POINT ( 'NONE',  ( -154.8505191518487152, -18.79705879280739467, -15.00000000000000000 ) ) ;
#11448 =( LENGTH_UNIT ( ) NAMED_UNIT ( * ) SI_UNIT ( .MILLI., .METRE. ) );
#11449 = CARTESIAN_POINT ( 'NONE',  ( 7.500000000000003553, -20.00000000000000000, -20.00000000000000000 ) ) ;
#11450 = ITEM_DEFINED_TRANSFORMATION ( 'NONE', 'NONE', #7796,  #10359 ) ;
#11451 = ORIENTED_EDGE ( 'NONE', *, *, #17782, .F. ) ;
#11452 = DIRECTION ( 'NONE',  ( 1.000000000000000000, 0.000000000000000000, 0.000000000000000000 ) ) ;
#11453 = ORIENTED_EDGE ( 'NONE', *, *, #16722, .F. ) ;
#11454 = ORIENTED_EDGE ( 'NONE', *, *, #13837, .T. ) ;
#11455 = DIRECTION ( 'NONE',  ( 0.000000000000000000, -0.000000000000000000, 1.000000000000000000 ) ) ;
#11456 = CARTESIAN_POINT ( 'NONE',  ( 0.1397371499201710277, 1.362866705336852169, -3.500000000000000000 ) ) ;
#11457 = CARTESIAN_POINT ( 'NONE',  ( 50.02271294988506156, 50.50051614449765935, -6.000000000000000888 ) ) ;
#11458 = PLANE ( 'NONE',  #15174 ) ;
#11459 = CARTESIAN_POINT ( 'NONE',  ( 4.175326769692855322, 2.060699556488906126, 3.569236330973482030 ) ) ;
#11460 = CARTESIAN_POINT ( 'NONE',  ( 48.02776887271745210, 49.39948385550241028, -5.992620115222778487 ) ) ;
#11461 = CARTESIAN_POINT ( 'NONE',  ( 19.76107906696393357, -23.08216711247132835, 0.000000000000000000 ) ) ;
#11462 = CARTESIAN_POINT ( 'NONE',  ( 54.13287192849676188, 46.29948385550240886, 5.649768623646098220 ) ) ;
#11463 = CARTESIAN_POINT ( 'NONE',  ( 56.81924384183006538, 46.80051614449766362, -4.924951120819380357 ) ) ;
#11464 = CARTESIAN_POINT ( 'NONE',  ( 2.000000000000000000, 1.773042676681340524, -2.059984127722458425E-15 ) ) ;
#11465 = DIRECTION ( 'NONE',  ( -0.000000000000000000, -0.000000000000000000, -1.000000000000000000 ) ) ;
#11466 = CARTESIAN_POINT ( 'NONE',  ( 6.207671477328021048, 3.321994320370322828, -4.246137054663353005 ) ) ;
#11467 = AXIS2_PLACEMENT_3D ( 'NONE', #17967, #10484, #48 ) ;
#11468 = ADVANCED_FACE ( 'NONE', ( #15157 ), #3302, .T. ) ;
#11469 = ORIENTED_EDGE ( 'NONE', *, *, #5576, .F. ) ;
#11470 = DIRECTION ( 'NONE',  ( 0.000000000000000000, 0.000000000000000000, 1.000000000000000000 ) ) ;
#11471 = ADVANCED_FACE ( 'NONE', ( #17827 ), #4386, .F. ) ;
#11472 = AXIS2_PLACEMENT_3D ( 'NONE', #9027, #14818, #7275 ) ;
#11473 = PRODUCT ( 'Mounting block', 'Mounting block', '', ( #13631 ) ) ;
#11474 = DIRECTION ( 'NONE',  ( -0.000000000000000000, -0.000000000000000000, -1.000000000000000000 ) ) ;
#11475 = CARTESIAN_POINT ( 'NONE',  ( 57.36023556966787851, 53.00051614449765225, 0.02388180880515038476 ) ) ;
#11476 = VECTOR ( 'NONE', #8155, 1000.000000000000000 ) ;
#11477 = CARTESIAN_POINT ( 'NONE',  ( -1.438549683741723797E-15, -3.375361811986503202, 1.153701847711634532 ) ) ;
#11478 = DIRECTION ( 'NONE',  ( 0.000000000000000000, 0.000000000000000000, 1.000000000000000000 ) ) ;
#11479 = EDGE_LOOP ( 'NONE', ( #5913, #9955, #12209, #6638 ) ) ;
#11480 = CARTESIAN_POINT ( 'NONE',  ( 2.899426713160750069, -23.82535289025860337, -9.999999999999994671 ) ) ;
#11481 = LINE ( 'NONE', #11682, #14005 ) ;
#11482 = CARTESIAN_POINT ( 'NONE',  ( 55.96859303347804371, 52.19948385550240033, 4.306917132069425946 ) ) ;
#11483 = CARTESIAN_POINT ( 'NONE',  ( -62.49999999999997158, 32.50000000000001421, -15.00000000000000000 ) ) ;
#11484 = CARTESIAN_POINT ( 'NONE',  ( 57.60143344285433642, 47.89948385550240317, -2.493737253992118319 ) ) ;
#11485 = CARTESIAN_POINT ( 'NONE',  ( 0.000000000000000000, 0.000000000000000000, -5.000000000000000000 ) ) ;
#11486 = CARTESIAN_POINT ( 'NONE',  ( 45.90387839640208512, 50.30051614449766362, -5.676469297603124353 ) ) ;
#11487 = CARTESIAN_POINT ( 'NONE',  ( -150.9999999999999716, -14.99999999999999645, -6.499999999999999112 ) ) ;
#11488 = CIRCLE ( 'NONE', #15901, 1.999999999999998224 ) ;
#11489 = CARTESIAN_POINT ( 'NONE',  ( 3.973110223767137850, -2.261493176400255405E-11, -3.565797985667433334 ) ) ;
#11490 = ORIENTED_EDGE ( 'NONE', *, *, #12182, .F. ) ;
#11491 = AXIS2_PLACEMENT_3D ( 'NONE', #12930, #13219, #5473 ) ;
#11492 = ORIENTED_EDGE ( 'NONE', *, *, #13598, .T. ) ;
#11493 = LINE ( 'NONE', #15480, #5944 ) ;
#11494 = AXIS2_PLACEMENT_3D ( 'NONE', #16234, #1044, #17807 ) ;
#11495 = ORIENTED_EDGE ( 'NONE', *, *, #18270, .F. ) ;
#11496 = CARTESIAN_POINT ( 'NONE',  ( -4.000000000000000000, 0.1981133338132459731, 2.096406544454392723E-17 ) ) ;
#11497 = EDGE_LOOP ( 'NONE', ( #10733, #2544 ) ) ;
#11498 = CARTESIAN_POINT ( 'NONE',  ( -57.64999999999994884, -14.99999999999998579, 15.00000000000000000 ) ) ;
#11499 = CARTESIAN_POINT ( 'NONE',  ( 56.66441430157296821, 60.09948385550240602, 2.141517661632100111 ) ) ;
#11500 = ORIENTED_EDGE ( 'NONE', *, *, #10711, .T. ) ;
#11501 = CARTESIAN_POINT ( 'NONE',  ( 8.500000000000000000, 0.000000000000000000, 0.000000000000000000 ) ) ;
#11502 = EDGE_LOOP ( 'NONE', ( #13601, #10967, #5053 ) ) ;
#11503 = VECTOR ( 'NONE', #5508, 1000.000000000000000 ) ;
#11504 = CARTESIAN_POINT ( 'NONE',  ( 45.27934281921075410, 61.29948385550240886, -6.458785618021043895 ) ) ;
#11505 = CARTESIAN_POINT ( 'NONE',  ( 3.355112389629172576, -2.681727112203168950, -0.2256878752776777242 ) ) ;
#11506 = AXIS2_PLACEMENT_3D ( 'NONE', #16095, #5400, #14509 ) ;
#11507 = CARTESIAN_POINT ( 'NONE',  ( 56.30877334542961421, 49.99948385550240459, -0.02388180880520959434 ) ) ;
#11508 = DIRECTION ( 'NONE',  ( 0.000000000000000000, 0.000000000000000000, -1.000000000000000000 ) ) ;
#11509 = CARTESIAN_POINT ( 'NONE',  ( -150.9999999999999716, -14.99999999999999645, 15.00000000000000000 ) ) ;
#11510 = CARTESIAN_POINT ( 'NONE',  ( 47.37792948025170858, 47.60051614449766078, 7.992620115222797139 ) ) ;
#11511 = CARTESIAN_POINT ( 'NONE',  ( 55.08986747509849380, 47.20051614449766220, 3.727524721679155384 ) ) ;
#11512 = COLOUR_RGB ( '',0.8941176470588234615, 0.8941176470588234615, 0.8941176470588234615 ) ;
#11513 = DIRECTION ( 'NONE',  ( -1.000000000000000000, 1.734723475976807094E-16, 0.000000000000000000 ) ) ;
#11514 = DIRECTION ( 'NONE',  ( 9.710251638871371392E-17, 5.969973981896233748E-17, 1.000000000000000000 ) ) ;
#11515 = ADVANCED_FACE ( 'NONE', ( #5142 ), #18408, .F. ) ;
#11516 = EDGE_LOOP ( 'NONE', ( #17897, #9825, #9018, #14145 ) ) ;
#11517 = ORIENTED_EDGE ( 'NONE', *, *, #772, .T. ) ;
#11518 = CARTESIAN_POINT ( 'NONE',  ( 0.3126073911696408136, 2.020725942163688060, 3.500000000000000000 ) ) ;
#11519 = PRESENTATION_STYLE_ASSIGNMENT (( #2983 ) ) ;
#11520 = ORIENTED_EDGE ( 'NONE', *, *, #14043, .T. ) ;
#11521 = CIRCLE ( 'NONE', #12161, 12.49999999999999645 ) ;
#11522 = CARTESIAN_POINT ( 'NONE',  ( 44.05948171654949874, 58.79948385550240886, 4.345558710429105354 ) ) ;
#11523 = SURFACE_SIDE_STYLE ('',( #19010 ) ) ;
#11524 = EDGE_LOOP ( 'NONE', ( #8952, #10663, #14081, #6506 ) ) ;
#11525 = ORIENTED_EDGE ( 'NONE', *, *, #5311, .F. ) ;
#11526 = DIRECTION ( 'NONE',  ( -1.000000000000000000, 0.000000000000000000, 0.000000000000000000 ) ) ;
#11527 = EDGE_LOOP ( 'NONE', ( #17462, #7214, #7049, #2240 ) ) ;
#11528 =( GEOMETRIC_REPRESENTATION_CONTEXT ( 3 ) GLOBAL_UNCERTAINTY_ASSIGNED_CONTEXT ( ( #2856 ) ) GLOBAL_UNIT_ASSIGNED_CONTEXT ( ( #11966, #14510, #1296 ) ) REPRESENTATION_CONTEXT ( 'NONE', 'WORKASPACE' ) );
#11529 = CARTESIAN_POINT ( 'NONE',  ( 0.08165819712376973238, 4.939961795957293234, 1.443735181952769064 ) ) ;
#11530 = VERTEX_POINT ( 'NONE', #11114 ) ;
#11531 = DIRECTION ( 'NONE',  ( 0.000000000000000000, 0.000000000000000000, -1.000000000000000000 ) ) ;
#11532 = CARTESIAN_POINT ( 'NONE',  ( 49.97728705011488159, 51.49948385550240459, -7.000000000000000888 ) ) ;
#11533 = CARTESIAN_POINT ( 'NONE',  ( 30.00000000000000355, -40.00000000000000000, 0.000000000000000000 ) ) ;
#11534 = ADVANCED_FACE ( 'NONE', ( #17121 ), #16929, .T. ) ;
#11535 = B_SPLINE_CURVE_WITH_KNOTS ( 'NONE', 3,
 ( #12605, #6629, #109, #8197, #6088 ),
 .UNSPECIFIED., .F., .F.,
 ( 4, 1, 4 ),
 ( 0.000000000000000000, 0.002886751345948128985, 0.005773502691896257970 ),
 .UNSPECIFIED. ) ;
#11536 = CARTESIAN_POINT ( 'NONE',  ( 47.74827507625469281, 50.40051614449764372, -7.007379884777203749 ) ) ;
#11537 = CYLINDRICAL_SURFACE ( 'NONE', #14544, 5.000000000000000888 ) ;
#11538 = AXIS2_PLACEMENT_3D ( 'NONE', #7816, #383, #10946 ) ;
#11539 = DIRECTION ( 'NONE',  ( -1.000000000000000000, 0.000000000000000000, 1.224646799147353207E-16 ) ) ;
#11540 = CARTESIAN_POINT ( 'NONE',  ( 0.02944718078426972890, -0.6813962075686093023, 3.500000000000000000 ) ) ;
#11541 = EDGE_CURVE ( 'NONE', #14564, #9381, #16970, .T. ) ;
#11542 = EDGE_CURVE ( 'NONE', #3214, #14841, #12594, .T. ) ;
#11543 =( GEOMETRIC_REPRESENTATION_CONTEXT ( 3 ) GLOBAL_UNCERTAINTY_ASSIGNED_CONTEXT ( ( #10670 ) ) GLOBAL_UNIT_ASSIGNED_CONTEXT ( ( #12129, #2245, #9851 ) ) REPRESENTATION_CONTEXT ( 'NONE', 'WORKASPACE' ) );
#11544 = ORIENTED_EDGE ( 'NONE', *, *, #1800, .T. ) ;
#11545 = ORIENTED_EDGE ( 'NONE', *, *, #1847, .T. ) ;
#11546 = CARTESIAN_POINT ( 'NONE',  ( 30.00000000000000000, -3.000000000000000000, -5.999999999999998224 ) ) ;
#11547 = LINE ( 'NONE', #14493, #13070 ) ;
#11548 = ORIENTED_EDGE ( 'NONE', *, *, #4018, .T. ) ;
#11549 = CYLINDRICAL_SURFACE ( 'NONE', #10505, 2.649999999999985700 ) ;
#11550 = CONICAL_SURFACE ( 'NONE', #5609, 1.610000000000000098, 0.7853981633974658205 ) ;
#11551 = ADVANCED_FACE ( 'NONE', ( #11022 ), #2117, .F. ) ;
#11552 = TOROIDAL_SURFACE ( 'NONE', #5611, 7.900000000000002132, 0.5999999999999979794 ) ;
#11553 = VERTEX_POINT ( 'NONE', #542 ) ;
#11554 = EDGE_LOOP ( 'NONE', ( #5382, #3718, #3114, #13976 ) ) ;
#11555 = DIRECTION ( 'NONE',  ( -0.6691306063588624564, 0.7431448254773903583, 0.000000000000000000 ) ) ;
#11556 = DIRECTION ( 'NONE',  ( 1.000000000000000000, 0.000000000000000000, 0.000000000000000000 ) ) ;
#11557 = CARTESIAN_POINT ( 'NONE',  ( 44.88205777487401349, 51.80051614449766362, 3.688883143319584779 ) ) ;
#11558 = FACE_OUTER_BOUND ( 'NONE', #18062, .T. ) ;
#11559 = FACE_OUTER_BOUND ( 'NONE', #5264, .T. ) ;
#11560 = CARTESIAN_POINT ( 'NONE',  ( 43.69122665457040000, 50.99948385550241170, 0.02388180880521036456 ) ) ;
#11561 = CARTESIAN_POINT ( 'NONE',  ( 4.071447262713888016, -2.020725942163694722, -3.499999999999999556 ) ) ;
#11562 = CARTESIAN_POINT ( 'NONE',  ( 52.29715082351547295, 48.39948385550240317, 6.992620115222774047 ) ) ;
#11563 = CIRCLE ( 'NONE', #14391, 15.00000000000000000 ) ;
#11564 = CARTESIAN_POINT ( 'NONE',  ( 42.38452918213190657, 45.90051614449766504, 2.450534656007115508 ) ) ;
#11565 = B_SPLINE_CURVE_WITH_KNOTS ( 'NONE', 3,
 ( #10709, #6114, #10797, #16614, #12085, #13560 ),
 .UNSPECIFIED., .F., .F.,
 ( 4, 2, 4 ),
 ( -3.640115492407174633E-06, 0.0002066546034006553863, 0.0004169493222937179812 ),
 .UNSPECIFIED. ) ;
#11566 = DIRECTION ( 'NONE',  ( 0.000000000000000000, 0.000000000000000000, -1.000000000000000000 ) ) ;
#11567 = EDGE_CURVE ( 'NONE', #1014, #4790, #16717, .T. ) ;
#11568 = PLANE ( 'NONE',  #868 ) ;
#11569 = SURFACE_SIDE_STYLE ('',( #13439 ) ) ;
#11570 = DIRECTION ( 'NONE',  ( 0.000000000000000000, 0.000000000000000000, 1.000000000000000000 ) ) ;
#11571 = CIRCLE ( 'NONE', #16607, 4.800000000000000711 ) ;
#11572 = ORIENTED_EDGE ( 'NONE', *, *, #15020, .T. ) ;
#11573 = CARTESIAN_POINT ( 'NONE',  ( 1.567478505476134606E-15, 4.618802153517012066, -3.433295621305382905 ) ) ;
#11574 = LINE ( 'NONE', #5801, #17863 ) ;
#11575 = CARTESIAN_POINT ( 'NONE',  ( 55.96859303347802239, 52.80051614449765651, -4.306917132069484566 ) ) ;
#11576 = AXIS2_PLACEMENT_3D ( 'NONE', #16157, #3830, #2166 ) ;
#11577 = FACE_OUTER_BOUND ( 'NONE', #15040, .T. ) ;
#11578 = DIRECTION ( 'NONE',  ( -1.000000000000000000, -0.000000000000000000, -0.000000000000000000 ) ) ;
#11579 = VECTOR ( 'NONE', #1188, 1000.000000000000000 ) ;
#11580 = ORIENTED_EDGE ( 'NONE', *, *, #5865, .F. ) ;
#11581 = VECTOR ( 'NONE', #14862, 1000.000000000000000 ) ;
#11582 = LINE ( 'NONE', #14520, #12032 ) ;
#11583 = ADVANCED_FACE ( 'NONE', ( #2222 ), #11613, .F. ) ;
#11584 = DIRECTION ( 'NONE',  ( 0.000000000000000000, -0.000000000000000000, 1.000000000000000000 ) ) ;
#11585 = CARTESIAN_POINT ( 'NONE',  ( 45.90387839640214196, 52.69948385550240033, 5.676469297603166098 ) ) ;
#11586 = DIRECTION ( 'NONE',  ( 0.000000000000000000, 0.000000000000000000, -1.000000000000000000 ) ) ;
#11587 = CARTESIAN_POINT ( 'NONE',  ( 49.97728705011486738, 49.49948385550241170, -8.000000000000001776 ) ) ;
#11588 = DIRECTION ( 'NONE',  ( 0.000000000000000000, 0.000000000000000000, 1.000000000000000000 ) ) ;
#11589 = EDGE_CURVE ( 'NONE', #228, #7385, #665, .T. ) ;
#11590 = CARTESIAN_POINT ( 'NONE',  ( 52.25172492374527877, 49.40051614449766504, 7.007379884777203749 ) ) ;
#11591 = DIRECTION ( 'NONE',  ( 0.000000000000000000, 0.000000000000000000, 1.000000000000000000 ) ) ;
#11592 = AXIS2_PLACEMENT_3D ( 'NONE', #15489, #17368, #1977 ) ;
#11593 = EDGE_LOOP ( 'NONE', ( #6260, #10829, #18046, #4355 ) ) ;
#11594 = CIRCLE ( 'NONE', #18823, 1.000000000000000000 ) ;
#11595 = VECTOR ( 'NONE', #13889, 1000.000000000000000 ) ;
#11596 = ORIENTED_EDGE ( 'NONE', *, *, #4492, .T. ) ;
#11597 = CARTESIAN_POINT ( 'NONE',  ( -154.9999999999999716, -14.99999999999999645, 17.00000000000000000 ) ) ;
#11598 = ORIENTED_EDGE ( 'NONE', *, *, #4544, .T. ) ;
#11599 = CARTESIAN_POINT ( 'NONE',  ( 5.130877905917027526, -0.6693483836014323396, 9.000000000000000000 ) ) ;
#11600 = CIRCLE ( 'NONE', #17882, 7.900000000000002132 ) ;
#11601 = ORIENTED_EDGE ( 'NONE', *, *, #6157, .T. ) ;
#11602 = CARTESIAN_POINT ( 'NONE',  ( -19.02113032590304442, -26.18033988749903074, -9.000000000000000000 ) ) ;
#11603 = ORIENTED_EDGE ( 'NONE', *, *, #1121, .F. ) ;
#11604 = CARTESIAN_POINT ( 'NONE',  ( 0.000000000000000000, 0.000000000000000000, -1.000000000000000000 ) ) ;
#11605 = ORIENTED_EDGE ( 'NONE', *, *, #2961, .F. ) ;
#11606 = CARTESIAN_POINT ( 'NONE',  ( 50.02271294988513972, 60.49948385550240459, 8.000000000000001776 ) ) ;
#11607 = AXIS2_PLACEMENT_3D ( 'NONE', #18340, #9575, #861 ) ;
#11608 = CARTESIAN_POINT ( 'NONE',  ( 8.500000000000000000, 2.886751345948123770, -5.000000000000000000 ) ) ;
#11609 = EDGE_CURVE ( 'NONE', #4928, #6411, #2023, .T. ) ;
#11610 = CARTESIAN_POINT ( 'NONE',  ( 55.69932041026404335, 47.89948385550240317, -1.875703265242203432 ) ) ;
#11611 = PLANE ( 'NONE',  #5084 ) ;
#11612 = DIRECTION ( 'NONE',  ( 0.000000000000000000, 0.000000000000000000, -1.000000000000000000 ) ) ;
#11613 = CONICAL_SURFACE ( 'NONE', #8181, 2.500000000000000888, 0.9599310885968785900 ) ;
#11614 = CARTESIAN_POINT ( 'NONE',  ( 52.62207051974829852, 48.60051614449766788, -7.992620115222797139 ) ) ;
#11615 = CARTESIAN_POINT ( 'NONE',  ( 56.30877334542961421, 49.00051614449765935, 0.02388180880515774693 ) ) ;
#11616 = CARTESIAN_POINT ( 'NONE',  ( -154.9999999999999716, -14.99999999999999645, 15.00000000000000000 ) ) ;
#11617 = CARTESIAN_POINT ( 'NONE',  ( -99.99999999999997158, -23.00000000000000711, -15.00000000000000000 ) ) ;
#11618 = ORIENTED_EDGE ( 'NONE', *, *, #13341, .T. ) ;
#11619 = ORIENTED_EDGE ( 'NONE', *, *, #17197, .F. ) ;
#11620 = DIRECTION ( 'NONE',  ( -1.000000000000000000, 0.000000000000000000, 0.000000000000000000 ) ) ;
#11621 = ORIENTED_EDGE ( 'NONE', *, *, #13030, .F. ) ;
#11622 = CARTESIAN_POINT ( 'NONE',  ( 43.33558569842703179, 57.09948385550240602, -2.141517661632099223 ) ) ;
#11623 = FACE_OUTER_BOUND ( 'NONE', #1327, .T. ) ;
#11624 = AXIS2_PLACEMENT_3D ( 'NONE', #17704, #1125, #13079 ) ;
#11625 = ORIENTED_EDGE ( 'NONE', *, *, #10992, .F. ) ;
#11626 = AXIS2_PLACEMENT_3D ( 'NONE', #6379, #3639, #15596 ) ;
#11627 = EDGE_LOOP ( 'NONE', ( #2813, #1543, #17526, #13847 ) ) ;
#11628 = CARTESIAN_POINT ( 'NONE',  ( -2.059999999999998721, 2.522772406243545965E-16, -0.3080913168122742518 ) ) ;
#11629 = DIRECTION ( 'NONE',  ( 0.000000000000000000, 0.5000000000000007772, -0.8660254037844381525 ) ) ;
#11630 = AXIS2_PLACEMENT_3D ( 'NONE', #4876, #12409, #7993 ) ;
#11631 = VERTEX_POINT ( 'NONE', #18695 ) ;
#11632 = CYLINDRICAL_SURFACE ( 'NONE', #3183, 1.000000000000000000 ) ;
#11633 = ORIENTED_EDGE ( 'NONE', *, *, #17924, .F. ) ;
#11634 = CARTESIAN_POINT ( 'NONE',  ( -1.243802165048909503, 3.900692638707381921, -3.223146290109805800 ) ) ;
#11635 = CARTESIAN_POINT ( 'NONE',  ( 56.66441430157296821, 52.09948385550240602, 2.141517661632100111 ) ) ;
#11636 = CYLINDRICAL_SURFACE ( 'NONE', #11168, 20.00000000000000000 ) ;
#11637 = CARTESIAN_POINT ( 'NONE',  ( 45.86712807150329496, 45.70051614449766220, 5.649768623646139964 ) ) ;
#11638 = CARTESIAN_POINT ( 'NONE',  ( 1.219878473194463187, -24.84890673354692936, 9.999999999999998224 ) ) ;
#11639 = DIRECTION ( 'NONE',  ( -0.000000000000000000, -0.000000000000000000, -1.000000000000000000 ) ) ;
#11640 = PRODUCT_DEFINITION_SHAPE ( 'NONE', 'NONE',  #19439 ) ;
#11641 = AXIS2_PLACEMENT_3D ( 'NONE', #9181, #8887, #4686 ) ;
#11642 = EDGE_LOOP ( 'NONE', ( #1722, #8980, #9983, #15779 ) ) ;
#11643 = ORIENTED_EDGE ( 'NONE', *, *, #8427, .T. ) ;
#11644 = CARTESIAN_POINT ( 'NONE',  ( 3.951447005078450037, 2.357513599190969256, -2.916666666666667407 ) ) ;
#11645 = DIRECTION ( 'NONE',  ( 1.000000000000000000, 0.000000000000000000, 0.000000000000000000 ) ) ;
#11646 = DIRECTION ( 'NONE',  ( 0.000000000000000000, 0.000000000000000000, -1.000000000000000000 ) ) ;
#11647 = DIRECTION ( 'NONE',  ( 0.000000000000000000, 0.000000000000000000, 1.000000000000000000 ) ) ;
#11648 = VERTEX_POINT ( 'NONE', #7984 ) ;
#11649 = CARTESIAN_POINT ( 'NONE',  ( 6.541171661047875396, 2.934678558896536504, 5.142480235691129664 ) ) ;
#11650 = AXIS2_PLACEMENT_3D ( 'NONE', #9240, #18099, #10719 ) ;
#11651 = VERTEX_POINT ( 'NONE', #5051 ) ;
#11652 = EDGE_LOOP ( 'NONE', ( #8570, #7651, #2733, #16689 ) ) ;
#11653 = EDGE_CURVE ( 'NONE', #9187, #18339, #15559, .T. ) ;
#11654 = DIRECTION ( 'NONE',  ( -0.000000000000000000, -0.000000000000000000, 1.000000000000000000 ) ) ;
#11655 = PRODUCT_DEFINITION_CONTEXT ( 'detailed design', #8651, 'design' ) ;
#11656 = APPLICATION_CONTEXT ( 'automotive_design' ) ;
#11657 = CARTESIAN_POINT ( 'NONE',  ( 43.69122665457040000, 48.00051614449766646, -0.02388180880515696977 ) ) ;
#11658 = CARTESIAN_POINT ( 'NONE',  ( 7.900000000000002132, 9.674709713264094059E-16, -7.900000000000002132 ) ) ;
#11659 = EDGE_CURVE ( 'NONE', #928, #7086, #14120, .T. ) ;
#11660 = DIRECTION ( 'NONE',  ( 1.000000000000000000, 0.000000000000000000, 0.000000000000000000 ) ) ;
#11661 = CARTESIAN_POINT ( 'NONE',  ( 44.30067958973596376, 52.89948385550241028, 1.875703265242204099 ) ) ;
#11662 = FACE_OUTER_BOUND ( 'NONE', #14142, .T. ) ;
#11663 = CARTESIAN_POINT ( 'NONE',  ( 45.86712807150323812, 53.29948385550240886, -5.649768623646098220 ) ) ;
#11664 = CARTESIAN_POINT ( 'NONE',  ( 58.41169779390614281, 49.00051614449765935, 0.02388180880515032231 ) ) ;
#11665 = EDGE_CURVE ( 'NONE', #12719, #15486, #5687, .T. ) ;
#11666 = CARTESIAN_POINT ( 'NONE',  ( 0.1983443223721553794, -3.359771601077102154, 4.180704885107414448 ) ) ;
#11667 = EDGE_CURVE ( 'NONE', #2621, #6553, #6616, .T. ) ;
#11668 = EDGE_LOOP ( 'NONE', ( #3674, #2708, #12493, #17109 ) ) ;
#11669 = DIRECTION ( 'NONE',  ( 1.000000000000000000, 0.000000000000000000, 0.000000000000000000 ) ) ;
#11670 = EDGE_CURVE ( 'NONE', #6724, #2159, #935, .T. ) ;
#11671 =( LENGTH_UNIT ( ) NAMED_UNIT ( * ) SI_UNIT ( .MILLI., .METRE. ) );
#11672 = AXIS2_PLACEMENT_3D ( 'NONE', #16296, #17670, #6005 ) ;
#11673 = ORIENTED_EDGE ( 'NONE', *, *, #14578, .T. ) ;
#11674 = CARTESIAN_POINT ( 'NONE',  ( -4.235886605889389145, -2.417314728048544303, -3.751161874094020909 ) ) ;
#11675 = DIRECTION ( 'NONE',  ( 1.000000000000000000, 0.000000000000000000, 0.000000000000000000 ) ) ;
#11676 = EDGE_CURVE ( 'NONE', #3708, #15661, #680, .T. ) ;
#11677 = CARTESIAN_POINT ( 'NONE',  ( -54.99999999999996447, -14.99999999999998579, -15.00000000000000000 ) ) ;
#11678 = EDGE_CURVE ( 'NONE', #18916, #6396, #17412, .T. ) ;
#11679 = LINE ( 'NONE', #10198, #17156 ) ;
#11680 = CARTESIAN_POINT ( 'NONE',  ( 6.367873360227556567, 2.886751345948125991, 4.999999999999999112 ) ) ;
#11681 = DIRECTION ( 'NONE',  ( 0.000000000000000000, 0.000000000000000000, 1.000000000000000000 ) ) ;
#11682 = CARTESIAN_POINT ( 'NONE',  ( 5.599999999999999645, 2.020725942163686284, -3.499999999999999556 ) ) ;
#11683 = CARTESIAN_POINT ( 'NONE',  ( 56.65037692655918988, 53.89948385550240317, -2.184720259617163762 ) ) ;
#11684 = DIRECTION ( 'NONE',  ( -1.734723475976807341E-16, -1.000000000000000000, 0.000000000000000000 ) ) ;
#11685 = CARTESIAN_POINT ( 'NONE',  ( 54.72065718078924590, 50.29948385550240886, 6.458785618021043895 ) ) ;
#11686 = CARTESIAN_POINT ( 'NONE',  ( 55.94051828345053679, 47.20051614449766220, 4.345558710429044069 ) ) ;
#11687 = FACE_OUTER_BOUND ( 'NONE', #18224, .T. ) ;
#11688 = ORIENTED_EDGE ( 'NONE', *, *, #19306, .F. ) ;
#11689 = ORIENTED_EDGE ( 'NONE', *, *, #16220, .T. ) ;
#11690 = CARTESIAN_POINT ( 'NONE',  ( 2.449293598294706513E-15, -20.00000000000000000, 9.000000000000000000 ) ) ;
#11691 = VERTEX_POINT ( 'NONE', #2318 ) ;
#11692 = CARTESIAN_POINT ( 'NONE',  ( -74.99999999999997158, 20.00000000000001421, 15.00000000000000000 ) ) ;
#11693 = VERTEX_POINT ( 'NONE', #17512 ) ;
#11694 = CARTESIAN_POINT ( 'NONE',  ( -18.00000000000000355, -19.99999999999999289, -12.00000000000000000 ) ) ;
#11695 = VERTEX_POINT ( 'NONE', #6904 ) ;
#11696 = DIRECTION ( 'NONE',  ( 1.000000000000000000, 0.000000000000000000, 0.000000000000000000 ) ) ;
#11697 = ORIENTED_EDGE ( 'NONE', *, *, #18659, .T. ) ;
#11698 = CARTESIAN_POINT ( 'NONE',  ( 57.60143344285433642, 61.89948385550241738, -2.493737253992118319 ) ) ;
#11699 = LINE ( 'NONE', #15938, #435 ) ;
#11700 = CARTESIAN_POINT ( 'NONE',  ( 46.45491332379572924, 49.29948385550240886, -4.840751629271157874 ) ) ;
#11701 = VECTOR ( 'NONE', #11002, 999.9999999999998863 ) ;
#11702 = CARTESIAN_POINT ( 'NONE',  ( 50.00000000000000000, 40.00000000000000000, 4.000000000000003553 ) ) ;
#11703 = LINE ( 'NONE', #15941, #6816 ) ;
#11704 = CARTESIAN_POINT ( 'NONE',  ( 43.34962307344078880, 64.10051614449766078, -2.184720259617096705 ) ) ;
#11705 = AXIS2_PLACEMENT_3D ( 'NONE', #13063, #5810, #2784 ) ;
#11706 = CARTESIAN_POINT ( 'NONE',  ( 51.97223112728249816, 46.60051614449764656, -5.992620115222793586 ) ) ;
#11707 = FACE_OUTER_BOUND ( 'NONE', #2038, .T. ) ;
#11708 = LINE ( 'NONE', #8964, #1892 ) ;
#11709 = ORIENTED_EDGE ( 'NONE', *, *, #12568, .T. ) ;
#11710 = ORIENTED_EDGE ( 'NONE', *, *, #9393, .T. ) ;
#11711 = CARTESIAN_POINT ( 'NONE',  ( 73.00000000000000000, 1.000000000000000000, 6.000000000000000000 ) ) ;
#11712 = VERTEX_POINT ( 'NONE', #5526 ) ;
#11713 = EDGE_CURVE ( 'NONE', #7579, #14564, #12893, .T. ) ;
#11714 = FACE_OUTER_BOUND ( 'NONE', #10223, .T. ) ;
#11715 = CARTESIAN_POINT ( 'NONE',  ( 2.449293598294706513E-15, -20.00000000000000000, 9.000000000000000000 ) ) ;
#11716 = ORIENTED_EDGE ( 'NONE', *, *, #6162, .F. ) ;
#11717 = ORIENTED_EDGE ( 'NONE', *, *, #17313, .F. ) ;
#11718 = AXIS2_PLACEMENT_3D ( 'NONE', #17879, #10695, #1307 ) ;
#11719 = CARTESIAN_POINT ( 'NONE',  ( -0.9999999999999995559, -15.10102051443364246, 9.000000000000000000 ) ) ;
#11720 = EDGE_CURVE ( 'NONE', #3828, #18807, #18087, .T. ) ;
#11721 = CARTESIAN_POINT ( 'NONE',  ( 54.09612160359786515, 47.69948385550240744, -5.676469297603166098 ) ) ;
#11722 = ORIENTED_EDGE ( 'NONE', *, *, #11678, .F. ) ;
#11723 = DIRECTION ( 'NONE',  ( 0.000000000000000000, 0.000000000000000000, 1.000000000000000000 ) ) ;
#11724 = ORIENTED_EDGE ( 'NONE', *, *, #11119, .F. ) ;
#11725 = CARTESIAN_POINT ( 'NONE',  ( 62.50000000000000000, 20.00000000000001421, 15.00000000000000000 ) ) ;
#11726 = AXIS2_PLACEMENT_3D ( 'NONE', #8878, #13290, #1342 ) ;
#11727 = CARTESIAN_POINT ( 'NONE',  ( 47.74827507625478518, 50.59948385550238470, 7.007379884777227730 ) ) ;
#11728 = DIRECTION ( 'NONE',  ( -0.000000000000000000, -0.000000000000000000, 1.000000000000000000 ) ) ;
#11729 = CARTESIAN_POINT ( 'NONE',  ( 54.09612160359792199, 49.30051614449765651, 5.676469297603124353 ) ) ;
#11730 = CARTESIAN_POINT ( 'NONE',  ( 3.951447005078448260, 1.347150628109122339, -3.499999999999999112 ) ) ;
#11731 = CARTESIAN_POINT ( 'NONE',  ( -13.86289650954791064, -6.617387872822862782, -9.000000000000000000 ) ) ;
#11732 = CONICAL_SURFACE ( 'NONE', #16765, 2.055000000000000160, 0.7853981633974400633 ) ;
#11733 = CARTESIAN_POINT ( 'NONE',  ( -4.204114297095464359, 1.660363174096617156, -3.602136431857887011 ) ) ;
#11734 = VECTOR ( 'NONE', #6738, 1000.000000000000000 ) ;
#11735 = ORIENTED_EDGE ( 'NONE', *, *, #2105, .T. ) ;
#11736 = ORIENTED_EDGE ( 'NONE', *, *, #7955, .T. ) ;
#11737 = DIRECTION ( 'NONE',  ( -0.000000000000000000, -0.000000000000000000, 1.000000000000000000 ) ) ;
#11738 = SURFACE_SIDE_STYLE ('',( #7043 ) ) ;
#11739 = CARTESIAN_POINT ( 'NONE',  ( 55.96859303347804371, 48.19948385550240033, 4.306917132069425946 ) ) ;
#11740 = CARTESIAN_POINT ( 'NONE',  ( 0.9999999999999997780, -6.008326913195983998, -0.8000000000000000444 ) ) ;
#11741 = EDGE_LOOP ( 'NONE', ( #6535, #18066, #11673, #3900 ) ) ;
#11742 = CARTESIAN_POINT ( 'NONE',  ( 0.000000000000000000, 0.000000000000000000, 0.000000000000000000 ) ) ;
#11743 = ORIENTED_EDGE ( 'NONE', *, *, #8244, .F. ) ;
#11744 = VERTEX_POINT ( 'NONE', #8271 ) ;
#11745 = CARTESIAN_POINT ( 'NONE',  ( -19.89043790736545603, -22.09056926535314602, -9.000000000000000000 ) ) ;
#11746 = DIRECTION ( 'NONE',  ( -0.000000000000000000, -0.000000000000000000, 1.000000000000000000 ) ) ;
#11747 = CARTESIAN_POINT ( 'NONE',  ( 55.08986747509849380, 47.20051614449766220, 3.727524721679155384 ) ) ;
#11748 = DIRECTION ( 'NONE',  ( 0.3090169943749560000, -0.9510565162951507556, 0.000000000000000000 ) ) ;
#11749 = CIRCLE ( 'NONE', #19298, 4.800000000000000711 ) ;
#11750 = DIRECTION ( 'NONE',  ( 0.000000000000000000, 0.000000000000000000, 1.000000000000000000 ) ) ;
#11751 = CARTESIAN_POINT ( 'NONE',  ( 46.49166364869460466, 58.69948385550240033, 4.867452303228209765 ) ) ;
#11752 = CARTESIAN_POINT ( 'NONE',  ( -150.9999999999999716, -14.99999999999999645, 15.00000000000000000 ) ) ;
#11753 = CARTESIAN_POINT ( 'NONE',  ( 43.33558569842703179, 55.09948385550241312, -2.141517661632099223 ) ) ;
#11754 = CARTESIAN_POINT ( 'NONE',  ( 42.39856655714564226, 50.10051614449766078, -2.493737253992044156 ) ) ;
#11755 = LINE ( 'NONE', #7063, #9369 ) ;
#11756 = CIRCLE ( 'NONE', #3325, 1.000000000000000444 ) ;
#11757 = CARTESIAN_POINT ( 'NONE',  ( 2.449293598294706513E-15, -20.00000000000000000, 15.00000000000000355 ) ) ;
#11758 = EDGE_CURVE ( 'NONE', #13102, #18690, #7197, .T. ) ;
#11759 = ORIENTED_EDGE ( 'NONE', *, *, #15670, .T. ) ;
#11760 = PRODUCT_RELATED_PRODUCT_CATEGORY ( 'part', '', ( #11800 ) ) ;
#11761 = CARTESIAN_POINT ( 'NONE',  ( -8.134732861516020819, -1.729090847147989773, -9.000000000000000000 ) ) ;
#11762 = CIRCLE ( 'NONE', #2387, 0.1000000000000002554 ) ;
#11763 = FACE_OUTER_BOUND ( 'NONE', #6536, .T. ) ;
#11764 = APPLICATION_CONTEXT ( 'automotive_design' ) ;
#11765 = DIRECTION ( 'NONE',  ( -0.000000000000000000, -0.000000000000000000, 1.000000000000000000 ) ) ;
#11766 = VECTOR ( 'NONE', #7641, 1000.000000000000000 ) ;
#11767 = CARTESIAN_POINT ( 'NONE',  ( 6.196878017913830305, 3.367876570272813730, 4.166666666666666075 ) ) ;
#11768 = CYLINDRICAL_SURFACE ( 'NONE', #5530, 2.649999999999985700 ) ;
#11769 = DIRECTION ( 'NONE',  ( 2.191393683118470056E-17, 7.538405132783724027E-17, 1.000000000000000000 ) ) ;
#11770 = EDGE_CURVE ( 'NONE', #3719, #1029, #3981, .T. ) ;
#11771 = DIRECTION ( 'NONE',  ( 1.000000000000000000, 0.000000000000000000, 0.000000000000000000 ) ) ;
#11772 = B_SPLINE_CURVE_WITH_KNOTS ( 'NONE', 3,
 ( #2321, #12896, #11505, #1128, #2624, #11318, #938, #1041 ),
 .UNSPECIFIED., .F., .F.,
 ( 4, 2, 2, 4 ),
 ( 2.465131517071610173E-07, 0.001183067374689837636, 0.001774477805458902699, 0.002365888236227967761 ),
 .UNSPECIFIED. ) ;
#11773 = CARTESIAN_POINT ( 'NONE',  ( 43.34962307344081012, 48.89948385550240317, 2.184720259617164650 ) ) ;
#11774 = EDGE_CURVE ( 'NONE', #5017, #442, #1169, .T. ) ;
#11775 = CARTESIAN_POINT ( 'NONE',  ( 3.999999999999999112, -1.539600717839012978, -3.300726591567080703 ) ) ;
#11776 = CIRCLE ( 'NONE', #11467, 4.000000000000003553 ) ;
#11777 = CARTESIAN_POINT ( 'NONE',  ( 45.27934281921075410, 55.29948385550240175, -6.458785618021043895 ) ) ;
#11778 = SURFACE_SIDE_STYLE ('',( #8560 ) ) ;
#11779 = CARTESIAN_POINT ( 'NONE',  ( 54.13287192849671214, 50.70051614449766220, -5.649768623646139964 ) ) ;
#11780 = DIRECTION ( 'NONE',  ( -0.000000000000000000, 0.000000000000000000, -1.000000000000000000 ) ) ;
#11782 = ORIENTED_EDGE ( 'NONE', *, *, #9021, .F. ) ;
#11781 = EDGE_CURVE ( 'NONE', #9743, #17840, #17319, .T. ) ;
#11783 = EDGE_CURVE ( 'NONE', #2523, #13933, #7120, .T. ) ;
#11784 = ORIENTED_EDGE ( 'NONE', *, *, #2825, .F. ) ;
#11785 = LINE ( 'NONE', #4251, #10104 ) ;
#11786 = VERTEX_POINT ( 'NONE', #14250 ) ;
#11787 = VECTOR ( 'NONE', #7001, 1000.000000000000000 ) ;
#11788 = FACE_OUTER_BOUND ( 'NONE', #3773, .T. ) ;
#11789 = VECTOR ( 'NONE', #16965, 1000.000000000000000 ) ;
#11790 = VERTEX_POINT ( 'NONE', #18795 ) ;
#11791 = DIRECTION ( 'NONE',  ( 0.000000000000000000, -1.000000000000000000, 0.000000000000000000 ) ) ;
#11792 = EDGE_CURVE ( 'NONE', #14634, #12719, #11315, .T. ) ;
#11793 = ORIENTED_EDGE ( 'NONE', *, *, #2450, .T. ) ;
#11794 = EDGE_CURVE ( 'NONE', #14477, #88, #3876, .T. ) ;
#11795 = LINE ( 'NONE', #17800, #226 ) ;
#11796 = ORIENTED_EDGE ( 'NONE', *, *, #16480, .F. ) ;
#11797 = CARTESIAN_POINT ( 'NONE',  ( 54.72065718078924590, 62.29948385550241596, 6.458785618021043895 ) ) ;
#11798 = CARTESIAN_POINT ( 'NONE',  ( 1.000000000000000444, -15.10102051443364246, -8.999999999999998224 ) ) ;
#11799 = CLOSED_SHELL ( 'NONE', ( #13836, #12811, #6739, #2363, #18905, #3428, #18941, #17728, #3590, #14301, #15424, #16736, #10284, #2720, #13948, #13105, #13123, #14581, #9038, #18416, #11515, #19139, #3182, #18183, #18736, #18883, #14287, #9737, #10412 ) ) ;
#11800 = PRODUCT ( 'driver roller', 'driver roller', '', ( #7749 ) ) ;
#11801 = CARTESIAN_POINT ( 'NONE',  ( 49.97728705011488870, 59.49948385550240459, -6.000000000000000888 ) ) ;
#11802 = EDGE_CURVE ( 'NONE', #8815, #2828, #5210, .T. ) ;
#11803 = DIRECTION ( 'NONE',  ( 0.000000000000000000, 1.000000000000000000, 0.000000000000000000 ) ) ;
#11804 = CARTESIAN_POINT ( 'NONE',  ( -6.259644161404860030E-16, -4.618802153517027165, -3.433295621305388234 ) ) ;
#11805 = CARTESIAN_POINT ( 'NONE',  ( 50.02271294988505446, 54.50051614449765935, -8.000000000000001776 ) ) ;
#11806 = CARTESIAN_POINT ( 'NONE',  ( 44.88205777487401349, 51.80051614449766362, 3.688883143319584779 ) ) ;
#11807 = AXIS2_PLACEMENT_3D ( 'NONE', #2295, #7174, #6976 ) ;
#11808 = DIRECTION ( 'NONE',  ( -1.000000000000000000, 0.000000000000000000, 0.000000000000000000 ) ) ;
#11809 = AXIS2_PLACEMENT_3D ( 'NONE', #5562, #7231, #13209 ) ;
#11810 = CARTESIAN_POINT ( 'NONE',  ( 2.449293598294706513E-15, -20.00000000000000000, 9.000000000000000000 ) ) ;
#11811 = VERTEX_POINT ( 'NONE', #9834 ) ;
#11812 = VERTEX_POINT ( 'NONE', #19193 ) ;
#11813 = DIRECTION ( 'NONE',  ( 0.000000000000000000, 0.000000000000000000, -1.000000000000000000 ) ) ;
#11814 = ORIENTED_EDGE ( 'NONE', *, *, #1388, .T. ) ;
#11815 = CARTESIAN_POINT ( 'NONE',  ( 42.63976443033212860, 64.99948385550240459, 0.02388180880522514787 ) ) ;
#11816 = FACE_OUTER_BOUND ( 'NONE', #11642, .T. ) ;
#11817 = VECTOR ( 'NONE', #19368, 1000.000000000000000 ) ;
#11818 = ORIENTED_EDGE ( 'NONE', *, *, #9328, .T. ) ;
#11819 = CARTESIAN_POINT ( 'NONE',  ( 5.560781378645575757, 0.000000000000000000, -4.000000000000000000 ) ) ;
#11820 = CARTESIAN_POINT ( 'NONE',  ( 56.65037692655918988, 45.89948385550240317, -2.184720259617163762 ) ) ;
#11821 = AXIS2_PLACEMENT_3D ( 'NONE', #7457, #7558, #6186 ) ;
#11822 = VERTEX_POINT ( 'NONE', #18987 ) ;
#11823 = DIRECTION ( 'NONE',  ( -1.000000000000000000, 0.000000000000000000, -0.000000000000000000 ) ) ;
#11824 = ORIENTED_EDGE ( 'NONE', *, *, #12996, .T. ) ;
#11825 = AXIS2_PLACEMENT_3D ( 'NONE', #13087, #10232, #19095 ) ;
#11826 = CARTESIAN_POINT ( 'NONE',  ( -3.158233816355059620, -39.56295201467614220, 9.000000000000000000 ) ) ;
#11827 = CARTESIAN_POINT ( 'NONE',  ( 52.25172492374522903, 59.59948385550240602, -7.007379884777225953 ) ) ;
#11828 = DIRECTION ( 'NONE',  ( -0.000000000000000000, 0.000000000000000000, -1.000000000000000000 ) ) ;
#11829 = CARTESIAN_POINT ( 'NONE',  ( 54.13287192849671214, 46.70051614449766220, -5.649768623646139964 ) ) ;
#11830 = DIRECTION ( 'NONE',  ( -1.000000000000000000, -0.000000000000000000, -0.000000000000000000 ) ) ;
#11831 = ADVANCED_FACE ( 'NONE', ( #15935 ), #5732, .F. ) ;
#11832 = CARTESIAN_POINT ( 'NONE',  ( -4.000000000000000000, 2.511478553582031203, -3.469254451724764543 ) ) ;
#11833 = EDGE_LOOP ( 'NONE', ( #4789, #11580 ) ) ;
#11834 = ADVANCED_FACE ( 'NONE', ( #2419 ), #8370, .F. ) ;
#11835 = AXIS2_PLACEMENT_3D ( 'NONE', #3340, #7929, #18256 ) ;
#11836 = VERTEX_POINT ( 'NONE', #7583 ) ;
#11837 = ORIENTED_EDGE ( 'NONE', *, *, #14592, .T. ) ;
#11838 = DIRECTION ( 'NONE',  ( -0.000000000000000000, -0.000000000000000000, 1.000000000000000000 ) ) ;
#11839 = CARTESIAN_POINT ( 'NONE',  ( 49.97728705011488159, 45.49948385550240459, -7.000000000000000888 ) ) ;
#11840 = CARTESIAN_POINT ( 'NONE',  ( 2.321707774797442170, -4.824281976789052351, -0.8000000000000000444 ) ) ;
#11841 = MECHANICAL_DESIGN_GEOMETRIC_PRESENTATION_REPRESENTATION (  '', ( #12237 ), #11528 ) ;
#11842 = ORIENTED_EDGE ( 'NONE', *, *, #16042, .T. ) ;
#11843 = CARTESIAN_POINT ( 'NONE',  ( -4.101948962585905356, -2.368261337751088824, -3.681124513963624167 ) ) ;
#11844 = ORIENTED_EDGE ( 'NONE', *, *, #8039, .T. ) ;
#11845 = ORIENTED_EDGE ( 'NONE', *, *, #17562, .F. ) ;
#11846 = CIRCLE ( 'NONE', #4022, 4.000000000000000000 ) ;
#11847 = FACE_OUTER_BOUND ( 'NONE', #637, .T. ) ;
#11848 = UNCERTAINTY_MEASURE_WITH_UNIT (LENGTH_MEASURE( 1.000000000000000082E-05 ), #9563, 'distance_accuracy_value', 'NONE');
#11849 = CARTESIAN_POINT ( 'NONE',  ( 50.00000000000000000, 40.00000000000000000, 0.000000000000000000 ) ) ;
#11850 = CARTESIAN_POINT ( 'NONE',  ( 46.49166364869456913, 46.30051614449766362, -4.867452303228181343 ) ) ;
#11851 = DIRECTION ( 'NONE',  ( 0.000000000000000000, 0.000000000000000000, 1.000000000000000000 ) ) ;
#11852 = CARTESIAN_POINT ( 'NONE',  ( 0.000000000000000000, 0.000000000000000000, -0.8000000000000000444 ) ) ;
#11853 = CARTESIAN_POINT ( 'NONE',  ( 44.30067958973596376, 58.89948385550241028, 1.875703265242204099 ) ) ;
#11854 = CARTESIAN_POINT ( 'NONE',  ( 3.522875095019493141, -2.820352903225631369, -3.598441714920572299 ) ) ;
#11855 = CARTESIAN_POINT ( 'NONE',  ( 45.90387839640214196, 50.69948385550240744, 5.676469297603166098 ) ) ;
#11856 = CARTESIAN_POINT ( 'NONE',  ( 54.72065718078918906, 56.70051614449766930, -6.458785618021089192 ) ) ;
#11857 = CARTESIAN_POINT ( 'NONE',  ( -154.9999999999999716, -14.99999999999999645, -6.499999999999999112 ) ) ;
#11858 = CARTESIAN_POINT ( 'NONE',  ( 13.99999999999999822, 0.000000000000000000, 0.000000000000000000 ) ) ;
#11859 = DIRECTION ( 'NONE',  ( 0.000000000000000000, 0.000000000000000000, 1.000000000000000000 ) ) ;
#11860 = PRESENTATION_LAYER_ASSIGNMENT (  '', '', ( #4964 ) ) ;
#11861 = DIRECTION ( 'NONE',  ( 2.775557561562891351E-17, 0.000000000000000000, -1.000000000000000000 ) ) ;
#11862 = ORIENTED_EDGE ( 'NONE', *, *, #6748, .T. ) ;
#11863 = DIRECTION ( 'NONE',  ( 0.000000000000000000, 0.000000000000000000, -1.000000000000000000 ) ) ;
#11864 = DIRECTION ( 'NONE',  ( -9.858538378746663627E-23, 5.031452844637890958E-23, -1.000000000000000000 ) ) ;
#11865 = AXIS2_PLACEMENT_3D ( 'NONE', #708, #9899, #9605 ) ;
#11866 = CARTESIAN_POINT ( 'NONE',  ( -7.499999999999998224, -20.00000000000000000, -20.00000000000000000 ) ) ;
#11867 = CARTESIAN_POINT ( 'NONE',  ( 1.000000000000000000, -5.408326913195983465, 0.000000000000000000 ) ) ;
#11868 = DIRECTION ( 'NONE',  ( 1.000000000000000000, -0.000000000000000000, -0.000000000000000000 ) ) ;
#11869 = AXIS2_PLACEMENT_3D ( 'NONE', #17609, #5625, #5823 ) ;
#11870 = DIRECTION ( 'NONE',  ( 1.000000000000000000, 0.000000000000000000, 0.000000000000000000 ) ) ;
#11871 = CIRCLE ( 'NONE', #8436, 20.00000000000000000 ) ;
#11872 = DIRECTION ( 'NONE',  ( -0.000000000000000000, -0.000000000000000000, -1.000000000000000000 ) ) ;
#11873 = CARTESIAN_POINT ( 'NONE',  ( 45.86712807150323812, 59.29948385550240175, -5.649768623646098220 ) ) ;
#11874 = DIRECTION ( 'NONE',  ( -0.000000000000000000, -0.000000000000000000, -1.000000000000000000 ) ) ;
#11875 = CARTESIAN_POINT ( 'NONE',  ( 54.72065718078924590, 56.29948385550240886, 6.458785618021043895 ) ) ;
#11876 = CARTESIAN_POINT ( 'NONE',  ( 1.000000000000000000, -14.00000000000000000, 8.999999999999998224 ) ) ;
#11877 = CARTESIAN_POINT ( 'NONE',  ( 54.13287192849671214, 52.70051614449766220, -5.649768623646139964 ) ) ;
#11878 = AXIS2_PLACEMENT_3D ( 'NONE', #6684, #14223, #17094 ) ;
#11879 = CARTESIAN_POINT ( 'NONE',  ( 0.000000000000000000, 0.4273491293402468805, 0.000000000000000000 ) ) ;
#11880 = EDGE_LOOP ( 'NONE', ( #12278, #2141, #14478, #18015, #15057, #18846, #14270, #17147, #19228 ) ) ;
#11881 = ORIENTED_EDGE ( 'NONE', *, *, #4229, .T. ) ;
#11882 = DIRECTION ( 'NONE',  ( -1.000000000000000000, 0.000000000000000000, -0.000000000000000000 ) ) ;
#11883 = ORIENTED_EDGE ( 'NONE', *, *, #4897, .F. ) ;
#11884 = VECTOR ( 'NONE', #1008, 999.9999999999998863 ) ;
#11885 = CYLINDRICAL_SURFACE ( 'NONE', #10611, 12.49999999999999645 ) ;
#11886 = ORIENTED_EDGE ( 'NONE', *, *, #13361, .F. ) ;
#11887 = CARTESIAN_POINT ( 'NONE',  ( -3.158233816355195955, -0.4370479853238878887, 9.000000000000000000 ) ) ;
#11888 = ORIENTED_EDGE ( 'NONE', *, *, #18278, .T. ) ;
#11889 = CIRCLE ( 'NONE', #9692, 4.599999999999999645 ) ;
#11890 = DIRECTION ( 'NONE',  ( -0.000000000000000000, 1.000000000000000000, -0.000000000000000000 ) ) ;
#11891 = VERTEX_POINT ( 'NONE', #13369 ) ;
#11892 = LINE ( 'NONE', #17903, #18076 ) ;
#11893 = CARTESIAN_POINT ( 'NONE',  ( -162.9999999999999716, -14.99999999999999645, -15.00000000000000000 ) ) ;
#11894 = EDGE_CURVE ( 'NONE', #3326, #7144, #10542, .T. ) ;
#11895 = CARTESIAN_POINT ( 'NONE',  ( 50.02271294988511841, 56.49948385550240459, 6.000000000000000888 ) ) ;
#11896 = FACE_BOUND ( 'NONE', #8573, .T. ) ;
#11897 =( NAMED_UNIT ( * ) SI_UNIT ( $, .STERADIAN. ) SOLID_ANGLE_UNIT ( ) );
#11898 = CARTESIAN_POINT ( 'NONE',  ( 42.38452918213190657, 55.90051614449766504, 2.450534656007115508 ) ) ;
#11899 = AXIS2_PLACEMENT_3D ( 'NONE', #3448, #6758, #790 ) ;
#11900 = CARTESIAN_POINT ( 'NONE',  ( 51.92680522751238925, 49.40051614449766504, 6.007379884777208190 ) ) ;
#11901 = EDGE_CURVE ( 'NONE', #5480, #3706, #3354, .T. ) ;
#11903 = AXIS2_PLACEMENT_3D ( 'NONE', #9873, #19026, #14579 ) ;
#11902 = FACE_OUTER_BOUND ( 'NONE', #14241, .T. ) ;
#11904 = CIRCLE ( 'NONE', #14410, 5.000000000000000888 ) ;
#11905 = CARTESIAN_POINT ( 'NONE',  ( -65.14999999999996305, 32.50000000000001421, 15.00000000000000000 ) ) ;
#11906 = ORIENTED_EDGE ( 'NONE', *, *, #2019, .T. ) ;
#11907 = EDGE_CURVE ( 'NONE', #10814, #248, #4753, .T. ) ;
#11908 = EDGE_CURVE ( 'NONE', #628, #8587, #8033, .T. ) ;
#11909 = VECTOR ( 'NONE', #10991, 1000.000000000000000 ) ;
#11910 = ORIENTED_EDGE ( 'NONE', *, *, #12040, .F. ) ;
#11911 = CARTESIAN_POINT ( 'NONE',  ( -18.68843350152494054, -12.87662627267948956, 9.000000000000000000 ) ) ;
#11912 = ORIENTED_EDGE ( 'NONE', *, *, #5559, .T. ) ;
#11913 = CARTESIAN_POINT ( 'NONE',  ( 52.29715082351547295, 62.39948385550239607, 6.992620115222774047 ) ) ;
#11914 = DIRECTION ( 'NONE',  ( -0.03668796685672145313, 0.9993267699245927949, 2.695122805014889898E-17 ) ) ;
#11915 = VERTEX_POINT ( 'NONE', #15130 ) ;
#11916 = CARTESIAN_POINT ( 'NONE',  ( 3.260336594487419859, -23.79080536174652494, -8.999999999999998224 ) ) ;
#11917 = DIRECTION ( 'NONE',  ( 1.000000000000000000, 0.000000000000000000, 0.000000000000000000 ) ) ;
#11918 = ORIENTED_EDGE ( 'NONE', *, *, #13828, .F. ) ;
#11919 = CONICAL_SURFACE ( 'NONE', #7225, 3.309499999999999886, 0.7853981633974407295 ) ;
#11920 = FACE_OUTER_BOUND ( 'NONE', #12320, .T. ) ;
#11921 = VECTOR ( 'NONE', #3516, 1000.000000000000000 ) ;
#11922 = ORIENTED_EDGE ( 'NONE', *, *, #15190, .F. ) ;
#11923 = CARTESIAN_POINT ( 'NONE',  ( 58.41169779390614281, 47.99948385550239038, -0.02388180880523160798 ) ) ;
#11924 = AXIS2_PLACEMENT_3D ( 'NONE', #13090, #19099, #16435 ) ;
#11925 = CARTESIAN_POINT ( 'NONE',  ( 4.000000000000000000, 2.309401076758497151, -5.000000000000000000 ) ) ;
#11926 = EDGE_CURVE ( 'NONE', #5237, #18188, #19032, .T. ) ;
#11927 = CARTESIAN_POINT ( 'NONE',  ( 57.36023556966787851, 55.99948385550239038, -0.02388180880522424582 ) ) ;
#11928 = FACE_BOUND ( 'NONE', #13674, .T. ) ;
#11929 = EDGE_CURVE ( 'NONE', #9042, #7605, #1515, .T. ) ;
#11930 = FACE_OUTER_BOUND ( 'NONE', #18722, .T. ) ;
#11931 = CARTESIAN_POINT ( 'NONE',  ( 50.02271294988505446, 56.50051614449766646, -7.000000000000000888 ) ) ;
#11932 = DIRECTION ( 'NONE',  ( 1.000000000000000000, 0.000000000000000000, 0.000000000000000000 ) ) ;
#11933 =( NAMED_UNIT ( * ) SI_UNIT ( $, .STERADIAN. ) SOLID_ANGLE_UNIT ( ) );
#11934 = DIRECTION ( 'NONE',  ( 1.000000000000000000, 0.000000000000000000, -0.000000000000000000 ) ) ;
#11935 = SHAPE_REPRESENTATION ( 'circlip for shafts normal_din_Circlip DIN 471 - 10 x 1', ( #10359 ), #11203 ) ;
#11936 = ORIENTED_EDGE ( 'NONE', *, *, #1841, .T. ) ;
#11937 = AXIS2_PLACEMENT_3D ( 'NONE', #19315, #8884, #9178 ) ;
#11938 = ORIENTED_EDGE ( 'NONE', *, *, #9614, .F. ) ;
#11939 = VERTEX_POINT ( 'NONE', #7676 ) ;
#11940 = CARTESIAN_POINT ( 'NONE',  ( 0.1085714285714285687, -3.798448662927795372, 0.000000000000000000 ) ) ;
#11941 =( LENGTH_UNIT ( ) NAMED_UNIT ( * ) SI_UNIT ( .MILLI., .METRE. ) );
#11942 = VECTOR ( 'NONE', #16313, 1000.000000000000000 ) ;
#11943 = CARTESIAN_POINT ( 'NONE',  ( 56.65037692655918988, 45.89948385550240317, -2.184720259617163762 ) ) ;
#11944 = AXIS2_PLACEMENT_3D ( 'NONE', #2504, #9820, #13258 ) ;
#11945 = DIRECTION ( 'NONE',  ( 0.000000000000000000, 0.000000000000000000, 1.000000000000000000 ) ) ;
#11946 = EDGE_LOOP ( 'NONE', ( #17838, #5240, #12418, #14953, #11331, #12587, #7488, #15826 ) ) ;
#11947 = CARTESIAN_POINT ( 'NONE',  ( 6.481779955677436256, 5.820445026626583918, -1.884471986315529758E-16 ) ) ;
#11948 = ORIENTED_EDGE ( 'NONE', *, *, #18145, .F. ) ;
#11949 = CARTESIAN_POINT ( 'NONE',  ( 56.66441430157294690, 56.90051614449766504, -2.141517661632166281 ) ) ;
#11950 = ORIENTED_EDGE ( 'NONE', *, *, #10362, .T. ) ;
#11951 = DIRECTION ( 'NONE',  ( 0.000000000000000000, 0.000000000000000000, 1.000000000000000000 ) ) ;
#11952 = CYLINDRICAL_SURFACE ( 'NONE', #8347, 1.000000000000000888 ) ;
#11953 = EDGE_CURVE ( 'NONE', #6947, #2794, #8762, .T. ) ;
#11954 = CARTESIAN_POINT ( 'NONE',  ( 43.69122665457040000, 56.00051614449765935, -0.02388180880515696977 ) ) ;
#11955 = DIRECTION ( 'NONE',  ( -0.000000000000000000, 1.000000000000000000, 1.224646799147353207E-16 ) ) ;
#11956 = EDGE_CURVE ( 'NONE', #14141, #2509, #5484, .T. ) ;
#11957 =( NAMED_UNIT ( * ) SI_UNIT ( $, .STERADIAN. ) SOLID_ANGLE_UNIT ( ) );
#11958 = AXIS2_PLACEMENT_3D ( 'NONE', #10160, #2832, #5856 ) ;
#11959 = CARTESIAN_POINT ( 'NONE',  ( 55.69932041026404335, 57.89948385550241028, -1.875703265242203432 ) ) ;
#11960 = CARTESIAN_POINT ( 'NONE',  ( -0.02448733951239248641, -4.877042772274742255, -3.751161874094027571 ) ) ;
#11961 = CARTESIAN_POINT ( 'NONE',  ( 54.09612160359786515, 51.69948385550240744, -5.676469297603166098 ) ) ;
#11962 = CARTESIAN_POINT ( 'NONE',  ( 45.31609314410960820, 54.30051614449765651, -6.485486291978072693 ) ) ;
#11963 = CARTESIAN_POINT ( 'NONE',  ( -18.68843350152494054, -12.87662627267948956, -9.000000000000000000 ) ) ;
#11964 = VERTEX_POINT ( 'NONE', #14840 ) ;
#11965 = FACE_OUTER_BOUND ( 'NONE', #2218, .T. ) ;
#11966 =( LENGTH_UNIT ( ) NAMED_UNIT ( * ) SI_UNIT ( .MILLI., .METRE. ) );
#11967 = CARTESIAN_POINT ( 'NONE',  ( -154.9999999999999716, -14.99999999999999645, 7.750000000000001776 ) ) ;
#11968 = ORIENTED_EDGE ( 'NONE', *, *, #13526, .F. ) ;
#11969 = FACE_OUTER_BOUND ( 'NONE', #8863, .T. ) ;
#11970 = EDGE_CURVE ( 'NONE', #16413, #12819, #8342, .T. ) ;
#11971 = DIRECTION ( 'NONE',  ( 1.000000000000000000, 0.000000000000000000, 0.000000000000000000 ) ) ;
#11972 = EDGE_CURVE ( 'NONE', #17166, #10122, #17996, .T. ) ;
#11973 = CARTESIAN_POINT ( 'NONE',  ( 55.94051828345050836, 61.79948385550240175, -4.345558710429103577 ) ) ;
#11974 = CARTESIAN_POINT ( 'NONE',  ( -154.9999999999999716, -14.99999999999999645, 6.499999999999999112 ) ) ;
#11975 = DIRECTION ( 'NONE',  ( -1.000000000000000000, 0.000000000000000000, 0.000000000000000000 ) ) ;
#11976 = LINE ( 'NONE', #8844, #11817 ) ;
#11977 = CARTESIAN_POINT ( 'NONE',  ( 56.65037692655918988, 55.89948385550240317, -2.184720259617163762 ) ) ;
#11978 = DIRECTION ( 'NONE',  ( 0.000000000000000000, 0.000000000000000000, 1.000000000000000000 ) ) ;
#11979 = CARTESIAN_POINT ( 'NONE',  ( 57.60143344285433642, 51.89948385550241028, -2.493737253992118319 ) ) ;
#11980 = DIRECTION ( 'NONE',  ( 1.000000000000000000, 0.000000000000000000, 0.000000000000000000 ) ) ;
#11981 = CARTESIAN_POINT ( 'NONE',  ( 47.74827507625469281, 56.40051614449766504, -7.007379884777203749 ) ) ;
#11982 = CARTESIAN_POINT ( 'NONE',  ( -54.99999999999996447, -14.99999999999998579, -15.00000000000000000 ) ) ;
#11983 = CARTESIAN_POINT ( 'NONE',  ( 0.000000000000000000, 0.5192545390863916310, 0.000000000000000000 ) ) ;
#11984 = EDGE_LOOP ( 'NONE', ( #3328, #2143 ) ) ;
#11985 =( LENGTH_UNIT ( ) NAMED_UNIT ( * ) SI_UNIT ( .MILLI., .METRE. ) );
#11986 = VERTEX_POINT ( 'NONE', #16519 ) ;
#11987 = FACE_OUTER_BOUND ( 'NONE', #9767, .T. ) ;
#11988 = ADVANCED_BREP_SHAPE_REPRESENTATION ( '', ( #2528, #10359 ), #14982 ) ;
#11989 = EDGE_LOOP ( 'NONE', ( #5841, #3870, #8169, #3204 ) ) ;
#11990 = CARTESIAN_POINT ( 'NONE',  ( -159.0000000000000000, -14.99999999999999645, 15.00000000000000000 ) ) ;
#11991 = CARTESIAN_POINT ( 'NONE',  ( 42.63976443033212860, 64.99948385550240459, 0.02388180880522514787 ) ) ;
#11992 = ORIENTED_EDGE ( 'NONE', *, *, #6163, .T. ) ;
#11993 = CARTESIAN_POINT ( 'NONE',  ( 1.655952806101427033, -3.662737355149048302, -1.182683869819604841E-14 ) ) ;
#11994 = ORIENTED_EDGE ( 'NONE', *, *, #16962, .F. ) ;
#11995 = PLANE ( 'NONE',  #9273 ) ;
#11996 = CARTESIAN_POINT ( 'NONE',  ( 2.449293598294706513E-15, -20.00000000000000000, -8.999999999999998224 ) ) ;
#11997 = CARTESIAN_POINT ( 'NONE',  ( 55.71335778527780747, 56.09948385550240602, 1.832500667257165983 ) ) ;
#11998 = FACE_BOUND ( 'NONE', #13148, .T. ) ;
#11999 = CARTESIAN_POINT ( 'NONE',  ( -19.97007065299860784, -21.09374499507130452, -9.000000000000000000 ) ) ;
#12000 = CARTESIAN_POINT ( 'NONE',  ( 56.81924384183006538, 50.80051614449766362, -4.924951120819380357 ) ) ;
#12001 = CARTESIAN_POINT ( 'NONE',  ( 46.49166364869456913, 56.30051614449766362, -4.867452303228181343 ) ) ;
#12002 = DIRECTION ( 'NONE',  ( 0.000000000000000000, 0.000000000000000000, 1.000000000000000000 ) ) ;
#12003 = FACE_BOUND ( 'NONE', #232, .T. ) ;
#12004 = ORIENTED_EDGE ( 'NONE', *, *, #2978, .T. ) ;
#12005 = ORIENTED_EDGE ( 'NONE', *, *, #12504, .F. ) ;
#12006 = CARTESIAN_POINT ( 'NONE',  ( 62.49999999999998579, 5.000000000000018652, 5.000000000000000000 ) ) ;
#12007 = VERTEX_POINT ( 'NONE', #17901 ) ;
#12008 = ADVANCED_FACE ( 'NONE', ( #16327 ), #7393, .F. ) ;
#12009 = CARTESIAN_POINT ( 'NONE',  ( -74.99999999999997158, 1.000000000000000000, 6.000000000000000000 ) ) ;
#12010 = CARTESIAN_POINT ( 'NONE',  ( 20.00000000000000000, -25.00000000000000711, -20.00000000000000000 ) ) ;
#12011 = ORIENTED_EDGE ( 'NONE', *, *, #18080, .F. ) ;
#12012 = DIRECTION ( 'NONE',  ( -1.000000000000000000, 0.000000000000000000, -0.000000000000000000 ) ) ;
#12013 = PRODUCT_DEFINITION ( 'UNKNOWN', '', #13555, #13984 ) ;
#12014 = DIRECTION ( 'NONE',  ( 0.000000000000000000, 0.000000000000000000, 1.000000000000000000 ) ) ;
#12015 = ORIENTED_EDGE ( 'NONE', *, *, #9073, .T. ) ;
#12016 = DIRECTION ( 'NONE',  ( 0.000000000000000000, 0.000000000000000000, -1.000000000000000000 ) ) ;
#12017 = VERTEX_POINT ( 'NONE', #7296 ) ;
#12018 = CARTESIAN_POINT ( 'NONE',  ( 42.39856655714564226, 64.10051614449766078, -2.493737253992044156 ) ) ;
#12019 = AXIS2_PLACEMENT_3D ( 'NONE', #9724, #18775, #5320 ) ;
#12020 = DIRECTION ( 'NONE',  ( -9.710251638871371392E-17, -5.969973981896233748E-17, -1.000000000000000000 ) ) ;
#12021 = EDGE_CURVE ( 'NONE', #5525, #1096, #11795, .T. ) ;
#12022 = ADVANCED_FACE ( 'NONE', ( #4461 ), #137, .T. ) ;
#12023 = CARTESIAN_POINT ( 'NONE',  ( 50.02271294988512551, 58.49948385550241170, 7.000000000000000888 ) ) ;
#12024 = DIRECTION ( 'NONE',  ( 0.000000000000000000, 0.000000000000000000, 1.000000000000000000 ) ) ;
#12025 = CARTESIAN_POINT ( 'NONE',  ( 0.1999999999999987899, 4.286263797015736595E-16, -3.500000000000000000 ) ) ;
#12026 = CARTESIAN_POINT ( 'NONE',  ( 56.65037692655921120, 55.10051614449766078, 2.184720259617097593 ) ) ;
#12027 = CARTESIAN_POINT ( 'NONE',  ( 3.806834918298644066, -4.553649124439118623E-15, -3.499999999999999556 ) ) ;
#12028 = ADVANCED_FACE ( 'NONE', ( #12089 ), #1709, .T. ) ;
#12029 = SURFACE_SIDE_STYLE ('',( #86 ) ) ;
#12030 = DIRECTION ( 'NONE',  ( -0.000000000000000000, -0.000000000000000000, 1.000000000000000000 ) ) ;
#12031 = ORIENTED_EDGE ( 'NONE', *, *, #12644, .F. ) ;
#12032 = VECTOR ( 'NONE', #6786, 999.9999999999998863 ) ;
#12033 = EDGE_LOOP ( 'NONE', ( #18622, #11204, #10295, #16561 ) ) ;
#12034 = APPLICATION_CONTEXT ( 'automotive_design' ) ;
#12035 = ORIENTED_EDGE ( 'NONE', *, *, #7733, .F. ) ;
#12036 = DIRECTION ( 'NONE',  ( 1.000000000000000000, 0.000000000000000000, 0.000000000000000000 ) ) ;
#12037 = VECTOR ( 'NONE', #18744, 1000.000000000000000 ) ;
#12038 = ADVANCED_FACE ( 'NONE', ( #8862 ), #1419, .T. ) ;
#12039 = CARTESIAN_POINT ( 'NONE',  ( 44.03140696652192787, 47.19948385550240744, -4.306917132069425058 ) ) ;
#12040 = EDGE_CURVE ( 'NONE', #15972, #4430, #714, .T. ) ;
#12041 = CARTESIAN_POINT ( 'NONE',  ( 2.000000000000000000, 1.773042676681340524, -2.059984127722458425E-15 ) ) ;
#12042 = ORIENTED_EDGE ( 'NONE', *, *, #8199, .T. ) ;
#12043 = CARTESIAN_POINT ( 'NONE',  ( -154.9999999999999716, -14.99999999999999645, -6.499999999999999112 ) ) ;
#12044 = ORIENTED_EDGE ( 'NONE', *, *, #1539, .F. ) ;
#12045 = CARTESIAN_POINT ( 'NONE',  ( 49.97728705011495265, 57.50051614449766646, 7.000000000000000888 ) ) ;
#12046 = ORIENTED_EDGE ( 'NONE', *, *, #18903, .F. ) ;
#12047 = EDGE_CURVE ( 'NONE', #13178, #3535, #11152, .T. ) ;
#12048 = FACE_OUTER_BOUND ( 'NONE', #7025, .T. ) ;
#12049 = UNCERTAINTY_MEASURE_WITH_UNIT (LENGTH_MEASURE( 1.000000000000000082E-05 ), #10080, 'distance_accuracy_value', 'NONE');
#12050 = CARTESIAN_POINT ( 'NONE',  ( 20.00000000000000000, -14.99999999999999289, -23.00000000000000000 ) ) ;
#12051 = CIRCLE ( 'NONE', #6726, 4.799999999999999822 ) ;
#12052 = CARTESIAN_POINT ( 'NONE',  ( 44.91013252490150620, 52.20051614449766220, -3.727524721679154940 ) ) ;
#12053 = DIRECTION ( 'NONE',  ( 0.000000000000000000, 0.000000000000000000, -1.000000000000000000 ) ) ;
#12054 = DIRECTION ( 'NONE',  ( 0.000000000000000000, 0.000000000000000000, 1.000000000000000000 ) ) ;
#12055 = CARTESIAN_POINT ( 'NONE',  ( 55.69932041026404335, 55.89948385550241028, -1.875703265242203432 ) ) ;
#12056 = AXIS2_PLACEMENT_3D ( 'NONE', #343, #4467, #16526 ) ;
#12057 = CARTESIAN_POINT ( 'NONE',  ( 42.39856655714564226, 54.10051614449766078, -2.493737253992044156 ) ) ;
#12058 = CARTESIAN_POINT ( 'NONE',  ( 6.362374563307726660, -5.433808049138435514, 0.8060918076010795685 ) ) ;
#12059 = DIRECTION ( 'NONE',  ( -0.000000000000000000, -0.000000000000000000, -1.000000000000000000 ) ) ;
#12060 = VERTEX_POINT ( 'NONE', #18671 ) ;
#12061 = DIRECTION ( 'NONE',  ( 0.000000000000000000, 0.000000000000000000, -1.000000000000000000 ) ) ;
#12062 = DIRECTION ( 'NONE',  ( 0.000000000000000000, 0.000000000000000000, -1.000000000000000000 ) ) ;
#12063 = VERTEX_POINT ( 'NONE', #6589 ) ;
#12064 = CARTESIAN_POINT ( 'NONE',  ( -62.49999999999997158, 40.00000000000001421, 0.000000000000000000 ) ) ;
#12065 = CARTESIAN_POINT ( 'NONE',  ( 19.02113032590313679, -26.18033988749876428, 9.000000000000000000 ) ) ;
#12066 = B_SPLINE_CURVE_WITH_KNOTS ( 'NONE', 3,
 ( #12933, #18938, #5477, #1666, #14885, #16756, #1356, #11947, #4510, #6161, #8904, #9193, #16566, #5979, #13522, #3324 ),
 .UNSPECIFIED., .F., .F.,
 ( 4, 3, 3, 3, 3, 4 ),
 ( 0.000000000000000000, 5.303647860849293065E-05, 0.0001057093501027226378, 0.0001642058037231607288, 0.0002210073443958831293, 0.0002236769549542879461 ),
 .UNSPECIFIED. ) ;
#12067 = CONICAL_SURFACE ( 'NONE', #13636, 4.000000000000000000, 0.8911886515913786111 ) ;
#12068 = CARTESIAN_POINT ( 'NONE',  ( 43.34962307344081012, 64.89948385550239607, 2.184720259617164650 ) ) ;
#12069 = CARTESIAN_POINT ( 'NONE',  ( 6.534838248920897819, 2.951765777552412651, 5.112608298763836601 ) ) ;
#12070 = CARTESIAN_POINT ( 'NONE',  ( 4.630153689607048761, 0.000000000000000000, 0.000000000000000000 ) ) ;
#12071 = CARTESIAN_POINT ( 'NONE',  ( 4.747884751462026820, -5.143694235355983579, -0.8000000000000000444 ) ) ;
#12072 = AXIS2_PLACEMENT_3D ( 'NONE', #1286, #12146, #9579 ) ;
#12073 = CARTESIAN_POINT ( 'NONE',  ( 47.70284917648453415, 61.39948385550241738, -6.992620115222774047 ) ) ;
#12074 = CARTESIAN_POINT ( 'NONE',  ( 30.00000000000000355, 40.00000000000000000, -9.999999999999998224 ) ) ;
#12075 = CARTESIAN_POINT ( 'NONE',  ( 49.97728705011486738, 51.49948385550240459, -8.000000000000001776 ) ) ;
#12076 = CARTESIAN_POINT ( 'NONE',  ( 2.000000000000000000, 1.773042676681340524, -2.059984127722458425E-15 ) ) ;
#12077 = CARTESIAN_POINT ( 'NONE',  ( 54.13287192849671214, 54.70051614449766220, -5.649768623646139964 ) ) ;
#12078 = EDGE_CURVE ( 'NONE', #8147, #6250, #10999, .T. ) ;
#12079 = DIRECTION ( 'NONE',  ( 0.9999419836444144449, 0.01077169184824096695, 0.000000000000000000 ) ) ;
#12080 = VECTOR ( 'NONE', #14177, 1000.000000000000000 ) ;
#12081 = EDGE_LOOP ( 'NONE', ( #2314, #12460 ) ) ;
#12082 = EDGE_CURVE ( 'NONE', #40, #6643, #2429, .T. ) ;
#12083 = ORIENTED_EDGE ( 'NONE', *, *, #14903, .T. ) ;
#12084 = MECHANICAL_DESIGN_GEOMETRIC_PRESENTATION_REPRESENTATION (  '', ( #15529 ), #15220 ) ;
#12085 = CARTESIAN_POINT ( 'NONE',  ( 1.567478505476135000E-15, 4.618802153517012954, -3.504269196027527844 ) ) ;
#12086 = ORIENTED_EDGE ( 'NONE', *, *, #5195, .F. ) ;
#12087 = DIRECTION ( 'NONE',  ( -1.000000000000000000, 0.000000000000000000, 0.000000000000000000 ) ) ;
#12088 = CARTESIAN_POINT ( 'NONE',  ( 54.09612160359786515, 61.69948385550240744, -5.676469297603166098 ) ) ;
#12089 = FACE_OUTER_BOUND ( 'NONE', #5731, .T. ) ;
#12090 = ORIENTED_EDGE ( 'NONE', *, *, #10836, .F. ) ;
#12091 = LINE ( 'NONE', #16521, #2093 ) ;
#12092 = DIRECTION ( 'NONE',  ( 0.000000000000000000, 0.000000000000000000, 1.000000000000000000 ) ) ;
#12093 = CARTESIAN_POINT ( 'NONE',  ( 55.11794222512601493, 54.19948385550241454, 3.688883143319541702 ) ) ;
#12094 = LINE ( 'NONE', #2003, #4643 ) ;
#12095 = DIRECTION ( 'NONE',  ( 0.000000000000000000, 0.000000000000000000, -1.000000000000000000 ) ) ;
#12096 = CARTESIAN_POINT ( 'NONE',  ( 54.72065718078918906, 54.70051614449765509, -6.458785618021089192 ) ) ;
#12097 = CARTESIAN_POINT ( 'NONE',  ( 46.45491332379576477, 55.70051614449766220, 4.840751629271188961 ) ) ;
#12098 = DIRECTION ( 'NONE',  ( 1.000000000000000000, 0.000000000000000000, 0.000000000000000000 ) ) ;
#12099 = CARTESIAN_POINT ( 'NONE',  ( 1.149999999999998135, 0.000000000000000000, 0.000000000000000000 ) ) ;
#12100 = VERTEX_POINT ( 'NONE', #12667 ) ;
#12101 = EDGE_LOOP ( 'NONE', ( #4286, #9784, #15683, #19327, #18407, #13383, #400, #16463 ) ) ;
#12102 = CARTESIAN_POINT ( 'NONE',  ( 6.207519134555854023, 1.039264565631282888, -4.999999999999109157 ) ) ;
#12103 = ORIENTED_EDGE ( 'NONE', *, *, #11067, .F. ) ;
#12104 = CARTESIAN_POINT ( 'NONE',  ( 44.03140696652192787, 63.19948385550240744, -4.306917132069425058 ) ) ;
#12105 = FACE_OUTER_BOUND ( 'NONE', #12682, .T. ) ;
#12106 = VERTEX_POINT ( 'NONE', #7960 ) ;
#12107 = DIRECTION ( 'NONE',  ( -0.000000000000000000, -0.000000000000000000, -1.000000000000000000 ) ) ;
#12108 = CARTESIAN_POINT ( 'NONE',  ( 56.66441430157296821, 46.09948385550240602, 2.141517661632100111 ) ) ;
#12109 = CLOSED_SHELL ( 'NONE', ( #12794, #12038, #17852, #174, #11179, #11534, #1510, #5188, #8548, #3872, #9372, #13993, #13118, #3532, #1424, #4850, #3203, #18330, #10593, #1956, #18042, #5201, #7126, #5730, #460, #4491, #15286 ) ) ;
#12110 = ORIENTED_EDGE ( 'NONE', *, *, #1250, .F. ) ;
#12111 = DIRECTION ( 'NONE',  ( 0.000000000000000000, 0.000000000000000000, 1.000000000000000000 ) ) ;
#12112 = ORIENTED_EDGE ( 'NONE', *, *, #14214, .T. ) ;
#12113 = CARTESIAN_POINT ( 'NONE',  ( 42.39856655714566358, 48.89948385550241028, 2.493737253992119207 ) ) ;
#12114 = CARTESIAN_POINT ( 'NONE',  ( 2.000000000000008882, 3.464101615137749945, 0.000000000000000000 ) ) ;
#12115 = AXIS2_PLACEMENT_3D ( 'NONE', #1326, #16621, #231 ) ;
#12116 = CARTESIAN_POINT ( 'NONE',  ( 44.03140696652192787, 57.19948385550238612, -4.306917132069425058 ) ) ;
#12117 = DIRECTION ( 'NONE',  ( 1.000000000000000000, 0.000000000000000000, 0.000000000000000000 ) ) ;
#12118 = CIRCLE ( 'NONE', #7111, 2.200000000000001066 ) ;
#12119 = CARTESIAN_POINT ( 'NONE',  ( 56.65037692655921120, 57.10051614449766078, 2.184720259617097593 ) ) ;
#12120 = CARTESIAN_POINT ( 'NONE',  ( -2.171643655288372443, 3.365003104552320767, 2.541098841762897165E-18 ) ) ;
#12121 = ADVANCED_FACE ( 'NONE', ( #12572 ), #9432, .F. ) ;
#12122 =( NAMED_UNIT ( * ) SI_UNIT ( $, .STERADIAN. ) SOLID_ANGLE_UNIT ( ) );
#12123 = FACE_OUTER_BOUND ( 'NONE', #10125, .T. ) ;
#12124 = ORIENTED_EDGE ( 'NONE', *, *, #11434, .F. ) ;
#12125 = ORIENTED_EDGE ( 'NONE', *, *, #16256, .F. ) ;
#12126 = AXIS2_PLACEMENT_3D ( 'NONE', #10405, #3075, #9133 ) ;
#12127 = ORIENTED_EDGE ( 'NONE', *, *, #19355, .T. ) ;
#12128 = CARTESIAN_POINT ( 'NONE',  ( 7.900000000000002132, 0.000000000000000000, 0.000000000000000000 ) ) ;
#12129 =( LENGTH_UNIT ( ) NAMED_UNIT ( * ) SI_UNIT ( .MILLI., .METRE. ) );
#12130 = AXIS2_PLACEMENT_3D ( 'NONE', #4332, #13250, #2881 ) ;
#12131 = CARTESIAN_POINT ( 'NONE',  ( 55.96859303347804371, 46.19948385550238612, 4.306917132069425946 ) ) ;
#12132 = DIRECTION ( 'NONE',  ( -0.000000000000000000, -0.000000000000000000, 1.000000000000000000 ) ) ;
#12133 = ORIENTED_EDGE ( 'NONE', *, *, #5452, .T. ) ;
#12134 = AXIS2_PLACEMENT_3D ( 'NONE', #2927, #12218, #7618 ) ;
#12135 = DIRECTION ( 'NONE',  ( 1.000000000000000000, 0.000000000000000000, 0.000000000000000000 ) ) ;
#12136 = ADVANCED_FACE ( 'NONE', ( #17004 ), #1904, .F. ) ;
#12137 = EDGE_LOOP ( 'NONE', ( #11130, #19011, #1265, #4308, #13391, #1536, #10336, #4654, #17005, #4645, #12186, #8681 ) ) ;
#12138 = CARTESIAN_POINT ( 'NONE',  ( 56.66441430157294690, 60.90051614449766504, -2.141517661632166281 ) ) ;
#12139 = ORIENTED_EDGE ( 'NONE', *, *, #15500, .T. ) ;
#12140 = LINE ( 'NONE', #18147, #10659 ) ;
#12141 = CARTESIAN_POINT ( 'NONE',  ( 2.449293598294706513E-15, -20.00000000000000000, -9.999999999999994671 ) ) ;
#12142 = CIRCLE ( 'NONE', #9007, 2.396904916527700102 ) ;
#12143 = CARTESIAN_POINT ( 'NONE',  ( 55.69932041026405045, 57.10051614449766788, 1.875703265242156359 ) ) ;
#12144 = CARTESIAN_POINT ( 'NONE',  ( -159.0000000000000000, -14.99999999999999645, 17.00000000000000000 ) ) ;
#12145 = EDGE_CURVE ( 'NONE', #8857, #5700, #13055, .T. ) ;
#12146 = DIRECTION ( 'NONE',  ( 0.000000000000000000, 0.000000000000000000, 1.000000000000000000 ) ) ;
#12147 = EDGE_CURVE ( 'NONE', #16750, #737, #9617, .T. ) ;
#12148 = EDGE_CURVE ( 'NONE', #18359, #4092, #8983, .T. ) ;
#12149 = CARTESIAN_POINT ( 'NONE',  ( 55.71335778527780747, 56.09948385550240602, 1.832500667257165983 ) ) ;
#12150 = CARTESIAN_POINT ( 'NONE',  ( -31.74999999999995737, 0.000000000000000000, 0.000000000000000000 ) ) ;
#12151 = CARTESIAN_POINT ( 'NONE',  ( 52.62207051974829852, 54.60051614449766788, -7.992620115222797139 ) ) ;
#12152 = CARTESIAN_POINT ( 'NONE',  ( -4.000000000000000000, 0.000000000000000000, 0.000000000000000000 ) ) ;
#12153 = DIRECTION ( 'NONE',  ( -1.000000000000000000, -0.000000000000000000, -0.000000000000000000 ) ) ;
#12154 = COLOUR_RGB ( '',0.8941176470588234615, 0.8941176470588234615, 0.8941176470588234615 ) ;
#12155 = ORIENTED_EDGE ( 'NONE', *, *, #14890, .T. ) ;
#12156 = FACE_OUTER_BOUND ( 'NONE', #3917, .T. ) ;
#12157 = EDGE_CURVE ( 'NONE', #189, #13316, #15611, .T. ) ;
#12158 = SHAPE_DEFINITION_REPRESENTATION ( #2748, #1926 ) ;
#12159 = ORIENTED_EDGE ( 'NONE', *, *, #9172, .F. ) ;
#12160 = DIRECTION ( 'NONE',  ( 1.000000000000000000, 0.000000000000000000, 0.000000000000000000 ) ) ;
#12161 = AXIS2_PLACEMENT_3D ( 'NONE', #9099, #12132, #7247 ) ;
#12162 = AXIS2_PLACEMENT_3D ( 'NONE', #9491, #9302, #10682 ) ;
#12163 = DIRECTION ( 'NONE',  ( 0.000000000000000000, -1.000000000000000000, -0.000000000000000000 ) ) ;
#12164 = CARTESIAN_POINT ( 'NONE',  ( 55.94051828345050836, 63.79948385550240886, -4.345558710429103577 ) ) ;
#12165 = CARTESIAN_POINT ( 'NONE',  ( 0.3126073911696399255, 2.020725942163686284, -3.499999999999999556 ) ) ;
#12166 = DIRECTION ( 'NONE',  ( 0.9999419836444144449, 0.01077169184824096695, 0.000000000000000000 ) ) ;
#12167 = EDGE_CURVE ( 'NONE', #8683, #1920, #15325, .T. ) ;
#12168 = CARTESIAN_POINT ( 'NONE',  ( 13.99999999999999822, 0.000000000000000000, 0.000000000000000000 ) ) ;
#12169 = ADVANCED_FACE ( 'NONE', ( #3557 ), #12285, .T. ) ;
#12170 = CARTESIAN_POINT ( 'NONE',  ( 52.29715082351547295, 56.39948385550238896, 6.992620115222774047 ) ) ;
#12171 = CARTESIAN_POINT ( 'NONE',  ( 4.000000000000000000, -1.084202172485504434E-14, -3.142992957459231906 ) ) ;
#12172 = CARTESIAN_POINT ( 'NONE',  ( 50.02271294988513972, 54.49948385550240459, 8.000000000000001776 ) ) ;
#12173 = DIRECTION ( 'NONE',  ( -0.000000000000000000, -0.000000000000000000, 1.000000000000000000 ) ) ;
#12174 = AXIS2_PLACEMENT_3D ( 'NONE', #14269, #18715, #15955 ) ;
#12175 = CARTESIAN_POINT ( 'NONE',  ( 56.66441430157294690, 54.90051614449765793, -2.141517661632166281 ) ) ;
#12176 = VECTOR ( 'NONE', #2539, 1000.000000000000000 ) ;
#12177 = CARTESIAN_POINT ( 'NONE',  ( -54.99999999999996447, -14.99999999999998579, 15.00000000000000000 ) ) ;
#12178 = ORIENTED_EDGE ( 'NONE', *, *, #5434, .F. ) ;
#12179 = CARTESIAN_POINT ( 'NONE',  ( -2.134523027080836115E-16, -0.3420925509533478404, -3.499999999999999112 ) ) ;
#12180 = CARTESIAN_POINT ( 'NONE',  ( 54.09612160359792199, 49.30051614449765651, 5.676469297603124353 ) ) ;
#12181 = VECTOR ( 'NONE', #10731, 1000.000000000000000 ) ;
#12182 = EDGE_CURVE ( 'NONE', #10423, #18115, #6685, .T. ) ;
#12183 = AXIS2_PLACEMENT_3D ( 'NONE', #16686, #7290, #13172 ) ;
#12184 = CARTESIAN_POINT ( 'NONE',  ( 75.00000000000000000, 32.50000000000001421, 9.999999999999998224 ) ) ;
#12185 = DIRECTION ( 'NONE',  ( -0.000000000000000000, -0.000000000000000000, -1.000000000000000000 ) ) ;
#12186 = ORIENTED_EDGE ( 'NONE', *, *, #82, .T. ) ;
#12187 = DIRECTION ( 'NONE',  ( -1.224646799147353207E-16, 0.000000000000000000, -1.000000000000000000 ) ) ;
#12188 = CYLINDRICAL_SURFACE ( 'NONE', #7320, 14.00000000000000000 ) ;
#12189 = EDGE_CURVE ( 'NONE', #9092, #7216, #10217, .T. ) ;
#12190 = CARTESIAN_POINT ( 'NONE',  ( 46.49166364869460466, 54.69948385550240033, 4.867452303228209765 ) ) ;
#12191 = DIRECTION ( 'NONE',  ( 0.000000000000000000, 0.000000000000000000, -1.000000000000000000 ) ) ;
#12192 = CYLINDRICAL_SURFACE ( 'NONE', #8280, 2.149999999999999023 ) ;
#12193 = VECTOR ( 'NONE', #5312, 1000.000000000000000 ) ;
#12194 = CARTESIAN_POINT ( 'NONE',  ( 45.27934281921082516, 55.70051614449766220, 6.458785618021089192 ) ) ;
#12195 = CARTESIAN_POINT ( 'NONE',  ( 44.88205777487401349, 55.80051614449766362, 3.688883143319584779 ) ) ;
#12196 = CARTESIAN_POINT ( 'NONE',  ( 1.747541505913279281, -3.837784562140273081, -3.503702292528912299 ) ) ;
#12197 = LINE ( 'NONE', #13667, #1588 ) ;
#12198 = VECTOR ( 'NONE', #4629, 1000.000000000000114 ) ;
#12199 = ORIENTED_EDGE ( 'NONE', *, *, #18385, .F. ) ;
#12200 = ORIENTED_EDGE ( 'NONE', *, *, #6261, .F. ) ;
#12201 = DIRECTION ( 'NONE',  ( 1.000000000000000000, 0.000000000000000000, 0.000000000000000000 ) ) ;
#12202 = EDGE_LOOP ( 'NONE', ( #10247, #1720 ) ) ;
#12203 = DIRECTION ( 'NONE',  ( -0.000000000000000000, -0.000000000000000000, 1.000000000000000000 ) ) ;
#12204 = VECTOR ( 'NONE', #149, 999.9999999999998863 ) ;
#12205 = ORIENTED_EDGE ( 'NONE', *, *, #7282, .T. ) ;
#12206 = CARTESIAN_POINT ( 'NONE',  ( 1.000000000000000000, -4.808326913195983821, 0.000000000000000000 ) ) ;
#12207 = CARTESIAN_POINT ( 'NONE',  ( 47.74827507625477807, 52.59948385550239891, 7.007379884777229506 ) ) ;
#12208 = EDGE_CURVE ( 'NONE', #1321, #16659, #5118, .T. ) ;
#12209 = ORIENTED_EDGE ( 'NONE', *, *, #15140, .T. ) ;
#12210 = FACE_OUTER_BOUND ( 'NONE', #14244, .T. ) ;
#12211 = ORIENTED_EDGE ( 'NONE', *, *, #2208, .T. ) ;
#12212 = CARTESIAN_POINT ( 'NONE',  ( 52.62207051974839089, 48.39948385550240317, 7.992620115222770494 ) ) ;
#12213 = AXIS2_PLACEMENT_3D ( 'NONE', #692, #18648, #2644 ) ;
#12214 = DIRECTION ( 'NONE',  ( 1.000000000000000000, 0.000000000000000000, 0.000000000000000000 ) ) ;
#12215 = EDGE_CURVE ( 'NONE', #18424, #206, #16804, .T. ) ;
#12216 = CARTESIAN_POINT ( 'NONE',  ( 43.34962307344081012, 56.89948385550240317, 2.184720259617164650 ) ) ;
#12217 = DIRECTION ( 'NONE',  ( -0.9781476007338065770, 0.2079116908177552348, 0.000000000000000000 ) ) ;
#12218 = DIRECTION ( 'NONE',  ( -1.000000000000000000, -0.000000000000000000, -0.000000000000000000 ) ) ;
#12219 = AXIS2_PLACEMENT_3D ( 'NONE', #16265, #8804, #1357 ) ;
#12220 = AXIS2_PLACEMENT_3D ( 'NONE', #4383, #10637, #7512 ) ;
#12221 = CARTESIAN_POINT ( 'NONE',  ( 50.02271294988505446, 54.50051614449765935, -7.000000000000000888 ) ) ;
#12222 = DIRECTION ( 'NONE',  ( -0.000000000000000000, -0.000000000000000000, 1.000000000000000000 ) ) ;
#12223 = CIRCLE ( 'NONE', #10972, 20.00000000000000000 ) ;
#12224 = CARTESIAN_POINT ( 'NONE',  ( 6.420058897733094128, -5.782965130189196223, 5.134498127650324400E-16 ) ) ;
#12225 = VERTEX_POINT ( 'NONE', #6395 ) ;
#12226 = ORIENTED_EDGE ( 'NONE', *, *, #9249, .T. ) ;
#12227 = ORIENTED_EDGE ( 'NONE', *, *, #11057, .T. ) ;
#12228 = FACE_OUTER_BOUND ( 'NONE', #14531, .T. ) ;
#12229 =( NAMED_UNIT ( * ) PLANE_ANGLE_UNIT ( ) SI_UNIT ( $, .RADIAN. ) );
#12230 = CIRCLE ( 'NONE', #17258, 0.9999999999999991118 ) ;
#12231 = CARTESIAN_POINT ( 'NONE',  ( 56.66441430157296821, 52.09948385550240602, 2.141517661632100111 ) ) ;
#12232 = FACE_OUTER_BOUND ( 'NONE', #877, .T. ) ;
#12233 = AXIS2_PLACEMENT_3D ( 'NONE', #12992, #19001, #12903 ) ;
#12234 = CIRCLE ( 'NONE', #17261, 5.899999999999999467 ) ;
#12235 = VERTEX_POINT ( 'NONE', #12372 ) ;
#12236 = CYLINDRICAL_SURFACE ( 'NONE', #14896, 4.000000000000031086 ) ;
#12237 = STYLED_ITEM ( 'NONE', ( #6004 ), #5922 ) ;
#12238 = ORIENTED_EDGE ( 'NONE', *, *, #2961, .T. ) ;
#12239 = CARTESIAN_POINT ( 'NONE',  ( 50.02271294988505446, 60.50051614449765935, -7.000000000000000888 ) ) ;
#12240 = VERTEX_POINT ( 'NONE', #18380 ) ;
#12241 = LINE ( 'NONE', #18247, #4108 ) ;
#12242 = UNCERTAINTY_MEASURE_WITH_UNIT (LENGTH_MEASURE( 1.000000000000000082E-05 ), #11671, 'distance_accuracy_value', 'NONE');
#12243 = DIRECTION ( 'NONE',  ( 1.000000000000000000, 0.000000000000000000, 0.000000000000000000 ) ) ;
#12244 = CARTESIAN_POINT ( 'NONE',  ( 44.91013252490150620, 58.20051614449766220, -3.727524721679154940 ) ) ;
#12245 = DIRECTION ( 'NONE',  ( -0.000000000000000000, -0.000000000000000000, -1.000000000000000000 ) ) ;
#12246 = DIRECTION ( 'NONE',  ( 0.000000000000000000, 0.000000000000000000, 1.000000000000000000 ) ) ;
#12247 = CARTESIAN_POINT ( 'NONE',  ( 55.69932041026404335, 63.89948385550240317, -1.875703265242203432 ) ) ;
#12248 = DIRECTION ( 'NONE',  ( 0.000000000000000000, -0.000000000000000000, -1.000000000000000000 ) ) ;
#12249 = VECTOR ( 'NONE', #1153, 1000.000000000000000 ) ;
#12250 = AXIS2_PLACEMENT_3D ( 'NONE', #18392, #348, #15050 ) ;
#12251 = CARTESIAN_POINT ( 'NONE',  ( 42.39856655714564226, 56.10051614449766078, -2.493737253992044156 ) ) ;
#12252 = ORIENTED_EDGE ( 'NONE', *, *, #2609, .F. ) ;
#12253 = DIRECTION ( 'NONE',  ( 1.000000000000000000, 0.000000000000000000, 0.000000000000000000 ) ) ;
#12254 = VERTEX_POINT ( 'NONE', #10896 ) ;
#12255 = DIRECTION ( 'NONE',  ( 0.000000000000000000, 0.000000000000000000, 1.000000000000000000 ) ) ;
#12256 = SHAPE_DEFINITION_REPRESENTATION ( #7101, #6546 ) ;
#12257 = ORIENTED_EDGE ( 'NONE', *, *, #4373, .F. ) ;
#12258 = CARTESIAN_POINT ( 'NONE',  ( 13.61000000000001009, 0.000000000000000000, 0.000000000000000000 ) ) ;
#12259 = EDGE_CURVE ( 'NONE', #11939, #17113, #843, .T. ) ;
#12260 = DIRECTION ( 'NONE',  ( 0.000000000000000000, 1.000000000000000000, 0.000000000000000000 ) ) ;
#12261 = CIRCLE ( 'NONE', #3819, 2.055000000000000160 ) ;
#12262 = EDGE_CURVE ( 'NONE', #15125, #3771, #2121, .T. ) ;
#12263 = EDGE_CURVE ( 'NONE', #11229, #10609, #16022, .T. ) ;
#12264 = CARTESIAN_POINT ( 'NONE',  ( 57.36023556966787851, 61.99948385550240459, -0.02388180880522424582 ) ) ;
#12265 = VECTOR ( 'NONE', #11296, 1000.000000000000000 ) ;
#12266 = CARTESIAN_POINT ( 'NONE',  ( 18.68843350152485527, -12.87662627267923909, 9.000000000000000000 ) ) ;
#12267 = DIRECTION ( 'NONE',  ( 1.000000000000000000, 0.000000000000000000, 0.000000000000000000 ) ) ;
#12268 = EDGE_CURVE ( 'NONE', #9631, #14352, #6419, .T. ) ;
#12269 = ADVANCED_FACE ( 'NONE', ( #5505 ), #7074, .F. ) ;
#12270 = CARTESIAN_POINT ( 'NONE',  ( 1.000000000000000000, -14.00000000000000000, 8.999999999999998224 ) ) ;
#12271 = CARTESIAN_POINT ( 'NONE',  ( 56.66441430157296821, 58.09948385550240602, 2.141517661632100111 ) ) ;
#12272 = CARTESIAN_POINT ( 'NONE',  ( 6.445127866599366762, 5.657054305385774917, 0.4229901806197435277 ) ) ;
#12273 = CARTESIAN_POINT ( 'NONE',  ( 43.18075615816989199, 61.19948385550241454, -4.924951120819313743 ) ) ;
#12274 = CARTESIAN_POINT ( 'NONE',  ( 44.03140696652198471, 55.80051614449766362, 4.306917132069485454 ) ) ;
#12275 = ADVANCED_FACE ( 'NONE', ( #17487 ), #19066, .F. ) ;
#12276 = CARTESIAN_POINT ( 'NONE',  ( -54.99999999999996447, -14.99999999999998579, 10.00000000000000000 ) ) ;
#12277 = DIRECTION ( 'NONE',  ( 1.000000000000000000, 0.000000000000000000, 0.000000000000000000 ) ) ;
#12278 = ORIENTED_EDGE ( 'NONE', *, *, #12384, .F. ) ;
#12279 = ADVANCED_FACE ( 'NONE', ( #18869 ), #11185, .T. ) ;
#12280 = EDGE_CURVE ( 'NONE', #8779, #18696, #5226, .T. ) ;
#12281 = CARTESIAN_POINT ( 'NONE',  ( -20.00000000000000000, -19.99999999999999289, -23.00000000000000000 ) ) ;
#12282 = CARTESIAN_POINT ( 'NONE',  ( 44.05948171654945611, 46.20051614449766220, -4.345558710429044069 ) ) ;
#12283 = CARTESIAN_POINT ( 'NONE',  ( 3.260336594487421635, -23.79080536174652494, 15.00000000000000355 ) ) ;
#12284 = AXIS2_PLACEMENT_3D ( 'NONE', #6910, #1043, #19200 ) ;
#12285 = PLANE ( 'NONE',  #4912 ) ;
#12286 = ORIENTED_EDGE ( 'NONE', *, *, #16122, .T. ) ;
#12287 = CARTESIAN_POINT ( 'NONE',  ( -19.02113032590304442, -26.18033988749903074, 9.000000000000000000 ) ) ;
#12288 = FACE_OUTER_BOUND ( 'NONE', #3292, .T. ) ;
#12289 = CARTESIAN_POINT ( 'NONE',  ( 55.08986747509849380, 45.20051614449766220, 3.727524721679155384 ) ) ;
#12290 = DIRECTION ( 'NONE',  ( -0.000000000000000000, -0.000000000000000000, -1.000000000000000000 ) ) ;
#12291 = FACE_BOUND ( 'NONE', #19129, .T. ) ;
#12292 =( REPRESENTATION_RELATIONSHIP ('NONE','NONE', #16703, #10550 ) REPRESENTATION_RELATIONSHIP_WITH_TRANSFORMATION ( #11450 )SHAPE_REPRESENTATION_RELATIONSHIP( ) );
#12293 = CARTESIAN_POINT ( 'NONE',  ( 54.68390685589039890, 59.30051614449766362, 6.485486291978072693 ) ) ;
#12294 = CARTESIAN_POINT ( 'NONE',  ( 56.30877334542961421, 57.00051614449766646, 0.02388180880515774693 ) ) ;
#12295 = DIRECTION ( 'NONE',  ( -1.224646799147353207E-16, 0.000000000000000000, -1.000000000000000000 ) ) ;
#12296 = CARTESIAN_POINT ( 'NONE',  ( 4.175813232069150338, -4.122719923832746325, 2.362127131240695889E-16 ) ) ;
#12297 = VERTEX_POINT ( 'NONE', #1201 ) ;
#12298 = ORIENTED_EDGE ( 'NONE', *, *, #3283, .F. ) ;
#12299 = CARTESIAN_POINT ( 'NONE',  ( 1.925929944387235853E-31, 15.00000000000001599, -9.999999999999998224 ) ) ;
#12300 = EDGE_LOOP ( 'NONE', ( #19302, #246, #13651, #18211 ) ) ;
#12301 = CARTESIAN_POINT ( 'NONE',  ( -8.134732861516020819, -1.729090847147989773, 9.000000000000000000 ) ) ;
#12302 = CARTESIAN_POINT ( 'NONE',  ( 43.34962307344078880, 56.10051614449766078, -2.184720259617096705 ) ) ;
#12303 = ORIENTED_EDGE ( 'NONE', *, *, #1556, .T. ) ;
#12304 = DIRECTION ( 'NONE',  ( 1.000000000000000000, 0.000000000000000000, 0.000000000000000000 ) ) ;
#12305 = CARTESIAN_POINT ( 'NONE',  ( 54.13287192849676188, 54.29948385550240886, 5.649768623646098220 ) ) ;
#12306 = ORIENTED_EDGE ( 'NONE', *, *, #3544, .F. ) ;
#12307 = CARTESIAN_POINT ( 'NONE',  ( -19.89043790736545603, -22.09056926535314602, 9.000000000000000000 ) ) ;
#12308 = EDGE_LOOP ( 'NONE', ( #10339, #12927, #5930, #15219 ) ) ;
#12309 = CARTESIAN_POINT ( 'NONE',  ( 52.57664461997811856, 47.59948385550239891, -8.007379884777229506 ) ) ;
#12310 = CARTESIAN_POINT ( 'NONE',  ( 52.95539523038642926, 45.00000000000002132, -5.827023132204991462 ) ) ;
#12311 = CARTESIAN_POINT ( 'NONE',  ( 52.25172492374522903, 61.59948385550239891, -7.007379884777225953 ) ) ;
#12312 = CARTESIAN_POINT ( 'NONE',  ( 5.599999999999999645, 3.061616997868383634E-16, -2.500000000000000444 ) ) ;
#12313 = FILL_AREA_STYLE ('',( #4781 ) ) ;
#12314 = CARTESIAN_POINT ( 'NONE',  ( 52.29715082351538769, 52.60051614449766788, -6.992620115222796251 ) ) ;
#12315 = DIRECTION ( 'NONE',  ( 0.000000000000000000, 0.000000000000000000, 1.000000000000000000 ) ) ;
#12316 = CARTESIAN_POINT ( 'NONE',  ( 56.66441430157296821, 54.09948385550240602, 2.141517661632100111 ) ) ;
#12317 = CARTESIAN_POINT ( 'NONE',  ( 6.385552186430389909, -5.773502691896263528, -1.564818079814629131E-31 ) ) ;
#12318 = EDGE_CURVE ( 'NONE', #6465, #6795, #17771, .T. ) ;
#12319 = ORIENTED_EDGE ( 'NONE', *, *, #13232, .T. ) ;
#12320 = EDGE_LOOP ( 'NONE', ( #16705, #18009, #8270, #5097, #4832, #3744, #1237, #14754 ) ) ;
#12321 = CARTESIAN_POINT ( 'NONE',  ( 14.86289650954800479, -33.38261212717704041, -9.000000000000000000 ) ) ;
#12322 = SURFACE_STYLE_USAGE ( .BOTH. , #13793 ) ;
#12323 = EDGE_CURVE ( 'NONE', #18844, #12414, #4302, .T. ) ;
#12324 = AXIS2_PLACEMENT_3D ( 'NONE', #14867, #10740, #1447 ) ;
#12325 = CARTESIAN_POINT ( 'NONE',  ( 50.02271294988512551, 52.49948385550240459, 7.000000000000000888 ) ) ;
#12326 = DIRECTION ( 'NONE',  ( -1.000000000000000000, 0.000000000000000000, 0.000000000000000000 ) ) ;
#12327 = VERTEX_POINT ( 'NONE', #8344 ) ;
#12328 = AXIS2_PLACEMENT_3D ( 'NONE', #2199, #12473, #2099 ) ;
#12329 = LINE ( 'NONE', #18430, #7697 ) ;
#12330 = VERTEX_POINT ( 'NONE', #13153 ) ;
#12331 = CARTESIAN_POINT ( 'NONE',  ( 42.63976443033212149, 60.00051614449765225, -0.02388180880514948964 ) ) ;
#12332 = ORIENTED_EDGE ( 'NONE', *, *, #16349, .T. ) ;
#12333 = DIRECTION ( 'NONE',  ( -1.000000000000000000, 0.000000000000000000, 0.000000000000000000 ) ) ;
#12334 = LINE ( 'NONE', #9199, #3061 ) ;
#12335 = CARTESIAN_POINT ( 'NONE',  ( 50.02271294988506156, 54.50051614449765935, -6.000000000000000888 ) ) ;
#12336 = CARTESIAN_POINT ( 'NONE',  ( 0.01055556052338940676, 4.084588180558400339, -2.925285743277528105 ) ) ;
#12337 = AXIS2_PLACEMENT_3D ( 'NONE', #6978, #1203, #8348 ) ;
#12338 = DIRECTION ( 'NONE',  ( -0.9135454576425982021, -0.4067366430758060925, 0.000000000000000000 ) ) ;
#12339 = CARTESIAN_POINT ( 'NONE',  ( 6.270568613849413886, 3.932080789230360196, -3.401571648088637101 ) ) ;
#12340 = CIRCLE ( 'NONE', #5784, 1.999999999999998224 ) ;
#12341 = CARTESIAN_POINT ( 'NONE',  ( 58.41169779390614281, 61.00051614449765935, 0.02388180880515032231 ) ) ;
#12342 = ORIENTED_EDGE ( 'NONE', *, *, #18456, .T. ) ;
#12343 = DIRECTION ( 'NONE',  ( -0.000000000000000000, 0.000000000000000000, -1.000000000000000000 ) ) ;
#12344 = FILL_AREA_STYLE ('',( #304 ) ) ;
#12345 = VERTEX_POINT ( 'NONE', #5313 ) ;
#12346 = CARTESIAN_POINT ( 'NONE',  ( 5.599999999999999645, 4.041451884327382338, 0.000000000000000000 ) ) ;
#12347 = CONTEXT_DEPENDENT_SHAPE_REPRESENTATION ( #17433, #14288 ) ;
#12348 = ORIENTED_EDGE ( 'NONE', *, *, #7114, .T. ) ;
#12349 = DIRECTION ( 'NONE',  ( -1.000000000000000000, 0.000000000000000000, -0.000000000000000000 ) ) ;
#12350 = DIRECTION ( 'NONE',  ( 0.1305261922200524616, -0.9914448613738103822, 0.000000000000000000 ) ) ;
#12351 = AXIS2_PLACEMENT_3D ( 'NONE', #104, #17857, #14895 ) ;
#12352 = CARTESIAN_POINT ( 'NONE',  ( 49.97728705011488159, 65.49948385550240459, -7.000000000000000888 ) ) ;
#12353 = DIRECTION ( 'NONE',  ( -0.000000000000000000, -0.000000000000000000, -1.000000000000000000 ) ) ;
#12354 = CARTESIAN_POINT ( 'NONE',  ( 45.60000000000000142, 0.000000000000000000, 2.055000000000000160 ) ) ;
#12355 = VECTOR ( 'NONE', #4845, 1000.000000000000000 ) ;
#12356 = CARTESIAN_POINT ( 'NONE',  ( -3.861362476283256129, -2.629030857716004199, -3.671615880910374941 ) ) ;
#12357 = CARTESIAN_POINT ( 'NONE',  ( 49.97728705011488159, 65.49948385550240459, -7.000000000000000888 ) ) ;
#12358 = CARTESIAN_POINT ( 'NONE',  ( -54.99999999999996447, -22.99999999999998579, 15.00000000000000000 ) ) ;
#12359 = CARTESIAN_POINT ( 'NONE',  ( 47.42335538002188144, 62.59948385550238470, 8.007379884777233059 ) ) ;
#12360 = ADVANCED_FACE ( 'NONE', ( #17593 ), #3751, .F. ) ;
#12361 = CARTESIAN_POINT ( 'NONE',  ( 45.90387839640208512, 58.30051614449766362, -5.676469297603124353 ) ) ;
#12362 = CARTESIAN_POINT ( 'NONE',  ( 0.000000000000000000, 0.000000000000000000, -4.694516984716113228 ) ) ;
#12363 = LINE ( 'NONE', #10792, #4103 ) ;
#12364 = VECTOR ( 'NONE', #8702, 1000.000000000000114 ) ;
#12365 = PRODUCT_RELATED_PRODUCT_CATEGORY ( 'part', '', ( #10075 ) ) ;
#12366 = EDGE_LOOP ( 'NONE', ( #5631, #10130, #4167, #2441 ) ) ;
#12367 = AXIS2_PLACEMENT_3D ( 'NONE', #3445, #16983, #12640 ) ;
#12368 = DIRECTION ( 'NONE',  ( 0.000000000000000000, 1.000000000000000000, 0.000000000000000000 ) ) ;
#12369 = CARTESIAN_POINT ( 'NONE',  ( 45.90387839640208512, 46.30051614449766362, -5.676469297603124353 ) ) ;
#12370 = CARTESIAN_POINT ( 'NONE',  ( 4.093692494532773729, -2.021783646005766766, 3.501831996793844493 ) ) ;
#12371 = ADVANCED_FACE ( 'NONE', ( #8641 ), #6875, .T. ) ;
#12372 = CARTESIAN_POINT ( 'NONE',  ( -162.9999999999999716, -14.99999999999999645, -10.00000000000000000 ) ) ;
#12373 = ORIENTED_EDGE ( 'NONE', *, *, #4258, .T. ) ;
#12374 = CARTESIAN_POINT ( 'NONE',  ( 32.49999999999998579, 40.00000000000001421, 5.000000000000002665 ) ) ;
#12375 = DIRECTION ( 'NONE',  ( 0.000000000000000000, -0.4999999999999991118, 0.8660254037844391517 ) ) ;
#12376 = B_SPLINE_CURVE_WITH_KNOTS ( 'NONE', 3,
 ( #18728, #18833, #18927, #11540, #7037, #5668 ),
 .UNSPECIFIED., .F., .F.,
 ( 4, 2, 4 ),
 ( 0.003805861006858101119, 0.004828937052660003254, 0.005852013098461904955 ),
 .UNSPECIFIED. ) ;
#12377 = CARTESIAN_POINT ( 'NONE',  ( 56.30877334542961421, 63.99948385550241170, -0.02388180880520959434 ) ) ;
#12378 = CYLINDRICAL_SURFACE ( 'NONE', #18114, 4.799999999999999822 ) ;
#12379 = CARTESIAN_POINT ( 'NONE',  ( 55.96859303347804371, 46.19948385550238612, 4.306917132069425946 ) ) ;
#12380 = CARTESIAN_POINT ( 'NONE',  ( 57.61547081786810764, 56.90051614449767214, -2.450534656007114176 ) ) ;
#12381 = CONICAL_SURFACE ( 'NONE', #13648, 3.500000000000000000, 1.047197551196600296 ) ;
#12382 = ADVANCED_FACE ( 'NONE', ( #2493 ), #15715, .T. ) ;
#12383 = CARTESIAN_POINT ( 'NONE',  ( 43.69122665457040000, 58.00051614449765935, -0.02388180880515696977 ) ) ;
#12384 = EDGE_CURVE ( 'NONE', #17210, #12106, #1801, .T. ) ;
#12385 = DIRECTION ( 'NONE',  ( 0.000000000000000000, 0.000000000000000000, 1.000000000000000000 ) ) ;
#12386 = CARTESIAN_POINT ( 'NONE',  ( -14.86289650954790886, -6.617387872822862782, 9.000000000000000000 ) ) ;
#12387 = ORIENTED_EDGE ( 'NONE', *, *, #12623, .F. ) ;
#12388 = AXIS2_PLACEMENT_3D ( 'NONE', #16071, #769, #11247 ) ;
#12389 = ORIENTED_EDGE ( 'NONE', *, *, #14534, .F. ) ;
#12390 = FACE_OUTER_BOUND ( 'NONE', #10919, .T. ) ;
#12391 = ORIENTED_EDGE ( 'NONE', *, *, #540, .F. ) ;
#12392 = EDGE_CURVE ( 'NONE', #13823, #1569, #12748, .T. ) ;
#12393 = DIRECTION ( 'NONE',  ( -1.000000000000000000, -1.387778780781445676E-16, 0.000000000000000000 ) ) ;
#12394 = EDGE_CURVE ( 'NONE', #3064, #9923, #1992, .T. ) ;
#12395 = ORIENTED_EDGE ( 'NONE', *, *, #7211, .F. ) ;
#12396 = DIRECTION ( 'NONE',  ( 0.000000000000000000, 0.000000000000000000, -1.000000000000000000 ) ) ;
#12397 = CARTESIAN_POINT ( 'NONE',  ( 44.05948171654949874, 50.79948385550239465, 4.345558710429104465 ) ) ;
#12398 = EDGE_CURVE ( 'NONE', #14377, #14662, #16199, .T. ) ;
#12399 = ORIENTED_EDGE ( 'NONE', *, *, #17899, .F. ) ;
#12400 = CARTESIAN_POINT ( 'NONE',  ( -0.3208286057739654917, 4.433571671609680465, -0.3503314178412548774 ) ) ;
#12401 = ORIENTED_EDGE ( 'NONE', *, *, #15391, .F. ) ;
#12402 = APPLICATION_CONTEXT ( 'automotive_design' ) ;
#12403 = CARTESIAN_POINT ( 'NONE',  ( 58.41169779390614281, 55.99948385550241170, -0.02388180880523160798 ) ) ;
#12404 = CARTESIAN_POINT ( 'NONE',  ( 2.449293598294706513E-15, -20.00000000000000000, 9.000000000000000000 ) ) ;
#12405 = CARTESIAN_POINT ( 'NONE',  ( 51.97223112728254790, 46.39948385550240317, 5.992620115222778487 ) ) ;
#12406 = DIRECTION ( 'NONE',  ( -9.858538378746663627E-23, 5.031452844637890958E-23, -1.000000000000000000 ) ) ;
#12407 = FILL_AREA_STYLE_COLOUR ( '', #13998 ) ;
#12408 = CARTESIAN_POINT ( 'NONE',  ( 52.29715082351538769, 58.60051614449766078, -6.992620115222796251 ) ) ;
#12409 = DIRECTION ( 'NONE',  ( -0.000000000000000000, -0.000000000000000000, -1.000000000000000000 ) ) ;
#12410 = CARTESIAN_POINT ( 'NONE',  ( 54.13287192849676188, 60.29948385550240886, 5.649768623646098220 ) ) ;
#12411 = CARTESIAN_POINT ( 'NONE',  ( 6.466260427357665819, -5.808561367196025671, 1.503437176544561004E-15 ) ) ;
#12412 = VECTOR ( 'NONE', #9154, 1000.000000000000000 ) ;
#12413 = VERTEX_POINT ( 'NONE', #7274 ) ;
#12414 = VERTEX_POINT ( 'NONE', #4234 ) ;
#12415 = DIRECTION ( 'NONE',  ( -0.3090169943749528914, 0.9510565162951518658, 0.000000000000000000 ) ) ;
#12416 = APPLICATION_PROTOCOL_DEFINITION ( 'draft international standard', 'automotive_design', 1998, #4879 ) ;
#12417 = CARTESIAN_POINT ( 'NONE',  ( 43.34962307344081012, 48.89948385550240317, 2.184720259617164650 ) ) ;
#12418 = ORIENTED_EDGE ( 'NONE', *, *, #16344, .T. ) ;
#12419 = CARTESIAN_POINT ( 'NONE',  ( -154.9999999999999716, -14.99999999999999645, 17.00000000000000000 ) ) ;
#12420 = AXIS2_PLACEMENT_3D ( 'NONE', #13846, #10800, #8051 ) ;
#12421 = VERTEX_POINT ( 'NONE', #1397 ) ;
#12422 = LINE ( 'NONE', #12621, #11921 ) ;
#12423 = ORIENTED_EDGE ( 'NONE', *, *, #15912, .T. ) ;
#12424 = CIRCLE ( 'NONE', #15568, 5.000000000000000888 ) ;
#12425 = EDGE_CURVE ( 'NONE', #8991, #17914, #13343, .T. ) ;
#12426 = DIRECTION ( 'NONE',  ( 0.000000000000000000, 0.000000000000000000, -1.000000000000000000 ) ) ;
#12427 = UNCERTAINTY_MEASURE_WITH_UNIT (LENGTH_MEASURE( 1.000000000000000082E-05 ), #15851, 'distance_accuracy_value', 'NONE');
#12428 = PLANE ( 'NONE',  #4624 ) ;
#12429 = CARTESIAN_POINT ( 'NONE',  ( 44.28664221472221385, 63.90051614449765793, 1.832500667257213722 ) ) ;
#12430 = DIRECTION ( 'NONE',  ( -0.000000000000000000, 0.000000000000000000, 1.000000000000000000 ) ) ;
#12431 = EDGE_CURVE ( 'NONE', #15728, #10416, #15891, .T. ) ;
#12432 = CARTESIAN_POINT ( 'NONE',  ( 20.00000000000000000, -25.00000000000000711, -23.00000000000000000 ) ) ;
#12433 = DIRECTION ( 'NONE',  ( -0.8090169943749487835, 0.5877852522924713607, 0.000000000000000000 ) ) ;
#12434 = CARTESIAN_POINT ( 'NONE',  ( 45.31609314410960820, 60.30051614449767072, -6.485486291978072693 ) ) ;
#12435 = VECTOR ( 'NONE', #11355, 1000.000000000000000 ) ;
#12436 = VERTEX_POINT ( 'NONE', #5712 ) ;
#12437 = ORIENTED_EDGE ( 'NONE', *, *, #15847, .T. ) ;
#12438 = DIRECTION ( 'NONE',  ( -1.000000000000000000, 0.000000000000000000, 0.000000000000000000 ) ) ;
#12439 = AXIS2_PLACEMENT_3D ( 'NONE', #4874, #16552, #6428 ) ;
#12440 = ORIENTED_EDGE ( 'NONE', *, *, #18036, .T. ) ;
#12441 = SURFACE_STYLE_FILL_AREA ( #7748 ) ;
#12442 = ORIENTED_EDGE ( 'NONE', *, *, #6152, .F. ) ;
#12443 = DIRECTION ( 'NONE',  ( 1.000000000000000000, 0.000000000000000000, 0.000000000000000000 ) ) ;
#12444 = FACE_OUTER_BOUND ( 'NONE', #11058, .T. ) ;
#12445 = ORIENTED_EDGE ( 'NONE', *, *, #9844, .F. ) ;
#12446 = AXIS2_PLACEMENT_3D ( 'NONE', #12168, #3172, #10497 ) ;
#12447 = FACE_OUTER_BOUND ( 'NONE', #12479, .T. ) ;
#12448 = UNCERTAINTY_MEASURE_WITH_UNIT (LENGTH_MEASURE( 1.000000000000000082E-05 ), #5376, 'distance_accuracy_value', 'NONE');
#12449 = CARTESIAN_POINT ( 'NONE',  ( -1.250000000000001110, 0.000000000000000000, -5.899999999999999467 ) ) ;
#12450 = LINE ( 'NONE', #1886, #12662 ) ;
#12451 = FACE_BOUND ( 'NONE', #2895, .T. ) ;
#12452 = CARTESIAN_POINT ( 'NONE',  ( 43.33558569842703179, 63.09948385550240602, -2.141517661632099223 ) ) ;
#12453 = FACE_OUTER_BOUND ( 'NONE', #948, .T. ) ;
#12454 = CARTESIAN_POINT ( 'NONE',  ( 45.27934281921075410, 61.29948385550240886, -6.458785618021043895 ) ) ;
#12455 = CARTESIAN_POINT ( 'NONE',  ( 43.34962307344078880, 58.10051614449766078, -2.184720259617096705 ) ) ;
#12456 = DIRECTION ( 'NONE',  ( 0.000000000000000000, 0.000000000000000000, 1.000000000000000000 ) ) ;
#12457 = DIRECTION ( 'NONE',  ( -0.000000000000000000, -0.000000000000000000, 1.000000000000000000 ) ) ;
#12458 = CIRCLE ( 'NONE', #7153, 5.000000000000000888 ) ;
#12459 = AXIS2_PLACEMENT_3D ( 'NONE', #19130, #11838, #12036 ) ;
#12460 = ORIENTED_EDGE ( 'NONE', *, *, #1388, .F. ) ;
#12461 = CARTESIAN_POINT ( 'NONE',  ( -65.14999999999996305, 32.50000000000001421, 15.00000000000000178 ) ) ;
#12462 = CARTESIAN_POINT ( 'NONE',  ( 6.481779955677444249, 2.910222513313288850, -5.040653254389421356 ) ) ;
#12463 = COLOUR_RGB ( '',1.000000000000000000, 0.9490196078431372140, 0.9098039215686274384 ) ;
#12464 = CYLINDRICAL_SURFACE ( 'NONE', #13457, 4.872650870659752442 ) ;
#12465 = DIRECTION ( 'NONE',  ( -1.000000000000000000, 0.000000000000000000, 0.000000000000000000 ) ) ;
#12466 = ORIENTED_EDGE ( 'NONE', *, *, #5446, .F. ) ;
#12467 = CARTESIAN_POINT ( 'NONE',  ( 32.00000000000000000, -1.000000000000000000, -5.999999999999998224 ) ) ;
#12468 = VECTOR ( 'NONE', #10438, 1000.000000000000000 ) ;
#12469 = CARTESIAN_POINT ( 'NONE',  ( 3.309651814758565180, -5.455921364805393026, -1.000000000000000000 ) ) ;
#12470 = CIRCLE ( 'NONE', #8733, 0.5999999999999998668 ) ;
#12471 = CARTESIAN_POINT ( 'NONE',  ( 51.97223112728254790, 60.39948385550241028, 5.992620115222778487 ) ) ;
#12472 = DIRECTION ( 'NONE',  ( 0.9989677110047502362, 0.04542589977017699732, -6.931730960091013400E-15 ) ) ;
#12473 = DIRECTION ( 'NONE',  ( 0.000000000000000000, 0.000000000000000000, 1.000000000000000000 ) ) ;
#12474 = CARTESIAN_POINT ( 'NONE',  ( 43.18075615816994173, 59.80051614449766362, 4.924951120819380357 ) ) ;
#12475 = CARTESIAN_POINT ( 'NONE',  ( 46.45491332379576477, 59.70051614449766220, 4.840751629271188961 ) ) ;
#12476 =( GEOMETRIC_REPRESENTATION_CONTEXT ( 3 ) GLOBAL_UNCERTAINTY_ASSIGNED_CONTEXT ( ( #19339 ) ) GLOBAL_UNIT_ASSIGNED_CONTEXT ( ( #8900, #5573, #2752 ) ) REPRESENTATION_CONTEXT ( 'NONE', 'WORKASPACE' ) );
#12477 = DIRECTION ( 'NONE',  ( 1.049727191973306010E-16, 0.5150380737757248584, -0.8571673013836862420 ) ) ;
#12478 = CARTESIAN_POINT ( 'NONE',  ( -4.000000000000000000, 2.309401076758498483, -5.000000000000000000 ) ) ;
#12479 = EDGE_LOOP ( 'NONE', ( #5043, #16418, #5680 ) ) ;
#12480 = EDGE_LOOP ( 'NONE', ( #2209, #18574, #6775, #17529 ) ) ;
#12481 = CARTESIAN_POINT ( 'NONE',  ( 6.245813541929285506, 1.036329910265332499, -5.105320956836708390 ) ) ;
#12482 = ORIENTED_EDGE ( 'NONE', *, *, #11659, .T. ) ;
#12483 = VECTOR ( 'NONE', #7292, 1000.000000000000000 ) ;
#12484 = AXIS2_PLACEMENT_3D ( 'NONE', #8172, #5422, #15927 ) ;
#12485 = CARTESIAN_POINT ( 'NONE',  ( 30.00000000000000355, 40.00000000000000000, 10.00000000000000000 ) ) ;
#12486 = ORIENTED_EDGE ( 'NONE', *, *, #7486, .T. ) ;
#12487 = CARTESIAN_POINT ( 'NONE',  ( -5.686050877451574337, -5.768780236673276995, 0.000000000000000000 ) ) ;
#12488 = ADVANCED_FACE ( 'NONE', ( #10299 ), #19265, .F. ) ;
#12489 = CARTESIAN_POINT ( 'NONE',  ( 56.66441430157296821, 52.09948385550240602, 2.141517661632100111 ) ) ;
#12490 = ORIENTED_EDGE ( 'NONE', *, *, #8644, .T. ) ;
#12491 =( GEOMETRIC_REPRESENTATION_CONTEXT ( 3 ) GLOBAL_UNCERTAINTY_ASSIGNED_CONTEXT ( ( #7731 ) ) GLOBAL_UNIT_ASSIGNED_CONTEXT ( ( #13743, #9228, #7669 ) ) REPRESENTATION_CONTEXT ( 'NONE', 'WORKASPACE' ) );
#12492 = CARTESIAN_POINT ( 'NONE',  ( 6.534838248920899595, -2.951765777552420644, -5.112608298763837489 ) ) ;
#12493 = ORIENTED_EDGE ( 'NONE', *, *, #11720, .F. ) ;
#12494 = CARTESIAN_POINT ( 'NONE',  ( 45.27934281921075410, 51.29948385550240175, -6.458785618021043895 ) ) ;
#12495 = CARTESIAN_POINT ( 'NONE',  ( 4.158807179406255550, 2.089320655794525639, -3.500000000000000000 ) ) ;
#12496 = EDGE_CURVE ( 'NONE', #8654, #12414, #11679, .T. ) ;
#12497 = CARTESIAN_POINT ( 'NONE',  ( 44.28664221472220675, 47.09948385550240602, -1.832500667257165317 ) ) ;
#12498 = FACE_OUTER_BOUND ( 'NONE', #17916, .T. ) ;
#12499 = LINE ( 'NONE', #7991, #13073 ) ;
#12500 = CARTESIAN_POINT ( 'NONE',  ( 42.63976443033212860, 62.00051614449764514, -0.02388180880514948964 ) ) ;
#12501 = VECTOR ( 'NONE', #11280, 1000.000000000000114 ) ;
#12502 = ADVANCED_FACE ( 'NONE', ( #18841 ), #5385, .T. ) ;
#12503 = CONICAL_SURFACE ( 'NONE', #2514, 3.500000000000000000, 1.047197551196600296 ) ;
#12504 = EDGE_CURVE ( 'NONE', #2538, #4669, #18935, .T. ) ;
#12505 = DIRECTION ( 'NONE',  ( -0.02045300604585054485, -0.9997908153927442809, -2.853726094247055479E-17 ) ) ;
#12506 = B_SPLINE_CURVE_WITH_KNOTS ( 'NONE', 3,
 ( #8424, #15984, #14305, #18654, #12840, #8530, #18848, #9889, #988, #10091, #8230, #12745, #16086, #6854, #792, #15888 ),
 .UNSPECIFIED., .F., .F.,
 ( 4, 3, 3, 3, 3, 4 ),
 ( 0.000000000000000000, 3.315506744709155554E-05, 6.608280158698769959E-05, 0.0001026520855291340739, 0.0001376952025664813454, 0.0001398064759190616429 ),
 .UNSPECIFIED. ) ;
#12507 = CARTESIAN_POINT ( 'NONE',  ( 47.74827507625478518, 56.59948385550238470, 7.007379884777227730 ) ) ;
#12508 = DIRECTION ( 'NONE',  ( 0.000000000000000000, 0.000000000000000000, -1.000000000000000000 ) ) ;
#12509 = DIRECTION ( 'NONE',  ( 1.000000000000000000, 0.000000000000000000, 0.000000000000000000 ) ) ;
#12510 = ORIENTED_EDGE ( 'NONE', *, *, #9233, .T. ) ;
#12511 = EDGE_CURVE ( 'NONE', #4089, #11530, #11547, .T. ) ;
#12512 = AXIS2_PLACEMENT_3D ( 'NONE', #11464, #5595, #11566 ) ;
#12513 = VERTEX_POINT ( 'NONE', #11449 ) ;
#12514 = CYLINDRICAL_SURFACE ( 'NONE', #18146, 2.000000000000001776 ) ;
#12515 = SURFACE_STYLE_FILL_AREA ( #14368 ) ;
#12516 = CARTESIAN_POINT ( 'NONE',  ( 47.74827507625478518, 52.59948385550239180, 7.007379884777227730 ) ) ;
#12517 = CYLINDRICAL_SURFACE ( 'NONE', #2798, 1.000000000000000888 ) ;
#12518 = ORIENTED_EDGE ( 'NONE', *, *, #10211, .F. ) ;
#12519 = VERTEX_POINT ( 'NONE', #16079 ) ;
#12520 = DIRECTION ( 'NONE',  ( 0.000000000000000000, 0.000000000000000000, 1.000000000000000000 ) ) ;
#12521 = AXIS2_PLACEMENT_3D ( 'NONE', #6097, #312, #13730 ) ;
#12522 = EDGE_CURVE ( 'NONE', #15831, #17166, #18104, .T. ) ;
#12523 = EDGE_CURVE ( 'NONE', #6643, #40, #9925, .T. ) ;
#12524 = ORIENTED_EDGE ( 'NONE', *, *, #58, .F. ) ;
#12525 = CARTESIAN_POINT ( 'NONE',  ( 55.96859303347802239, 62.80051614449766362, -4.306917132069484566 ) ) ;
#12526 = AXIS2_PLACEMENT_3D ( 'NONE', #12487, #4772, #18405 ) ;
#12527 = ORIENTED_EDGE ( 'NONE', *, *, #167, .F. ) ;
#12528 = CARTESIAN_POINT ( 'NONE',  ( 56.65037692655918988, 45.89948385550240317, -2.184720259617163762 ) ) ;
#12529 = PLANE ( 'NONE',  #10854 ) ;
#12530 = AXIS2_PLACEMENT_3D ( 'NONE', #18708, #14555, #12705 ) ;
#12531 = CARTESIAN_POINT ( 'NONE',  ( 44.28664221472221385, 59.90051614449767214, 1.832500667257213722 ) ) ;
#12532 = DIRECTION ( 'NONE',  ( -0.000000000000000000, -0.000000000000000000, 1.000000000000000000 ) ) ;
#12533 = LINE ( 'NONE', #293, #2392 ) ;
#12534 = CARTESIAN_POINT ( 'NONE',  ( 25.00000000000000711, -20.00000000000000000, -23.00000000000000000 ) ) ;
#12535 = AXIS2_PLACEMENT_3D ( 'NONE', #2855, #10090, #14499 ) ;
#12536 = CARTESIAN_POINT ( 'NONE',  ( 56.81924384183006538, 58.80051614449766362, -4.924951120819380357 ) ) ;
#12537 = CIRCLE ( 'NONE', #5976, 5.560781378645573980 ) ;
#12538 = TOROIDAL_SURFACE ( 'NONE', #7853, 5.000000000000000000, 0.5999999999999999778 ) ;
#12539 = ORIENTED_EDGE ( 'NONE', *, *, #8107, .F. ) ;
#12540 = EDGE_LOOP ( 'NONE', ( #1724, #4163, #8100, #1298, #3799, #11492, #13613, #13308, #5269, #12565, #14455, #6504 ) ) ;
#12541 = CARTESIAN_POINT ( 'NONE',  ( 0.4465819873852039379, 5.773502691896261751, 3.331019006688249527E-17 ) ) ;
#12542 = DIRECTION ( 'NONE',  ( 0.000000000000000000, 0.000000000000000000, 1.000000000000000000 ) ) ;
#12543 = ITEM_DEFINED_TRANSFORMATION ( 'NONE', 'NONE', #3857,  #10359 ) ;
#12544 = CIRCLE ( 'NONE', #3776, 2.499999999999999556 ) ;
#12545 = ORIENTED_EDGE ( 'NONE', *, *, #11327, .F. ) ;
#12546 = DIRECTION ( 'NONE',  ( 1.000000000000000000, 0.000000000000000000, 0.000000000000000000 ) ) ;
#12547 = DIRECTION ( 'NONE',  ( -1.000000000000000000, 0.000000000000000000, 0.000000000000000000 ) ) ;
#12549 = ADVANCED_FACE ( 'NONE', ( #17556 ), #18413, .T. ) ;
#12548 = ORIENTED_EDGE ( 'NONE', *, *, #7720, .T. ) ;
#12550 = CIRCLE ( 'NONE', #6598, 3.800000000000000266 ) ;
#12551 = EDGE_CURVE ( 'NONE', #3254, #12436, #19231, .T. ) ;
#12552 = DIRECTION ( 'NONE',  ( -0.000000000000000000, -0.000000000000000000, 1.000000000000000000 ) ) ;
#12553 = FACE_OUTER_BOUND ( 'NONE', #9189, .T. ) ;
#12554 = CONICAL_SURFACE ( 'NONE', #8151, 2.500000000000000888, 0.9599310885968785900 ) ;
#12555 = AXIS2_PLACEMENT_3D ( 'NONE', #7594, #12098, #13855 ) ;
#12556 = LINE ( 'NONE', #18655, #15792 ) ;
#12557 = CARTESIAN_POINT ( 'NONE',  ( -1.566204647097437563, -6.822536405429463713, -0.8000000000000000444 ) ) ;
#12558 = CARTESIAN_POINT ( 'NONE',  ( 56.30877334542961421, 45.99948385550240459, -0.02388180880520959434 ) ) ;
#12559 = CARTESIAN_POINT ( 'NONE',  ( -2.141980652367355020, -6.189445006155633422, -0.8000000000000000444 ) ) ;
#12560 = CARTESIAN_POINT ( 'NONE',  ( 43.18075615816989199, 57.19948385550241454, -4.924951120819313743 ) ) ;
#12561 = CARTESIAN_POINT ( 'NONE',  ( 42.63976443033212860, 60.00051614449764514, -0.02388180880514948964 ) ) ;
#12562 = CARTESIAN_POINT ( 'NONE',  ( -62.49999999999997158, 32.50000000000001421, 15.00000000000000000 ) ) ;
#12563 = ADVANCED_FACE ( 'NONE', ( #8314 ), #13699, .T. ) ;
#12564 = CIRCLE ( 'NONE', #14111, 5.400000000000000355 ) ;
#12565 = ORIENTED_EDGE ( 'NONE', *, *, #4680, .F. ) ;
#12566 = VECTOR ( 'NONE', #5108, 1000.000000000000000 ) ;
#12567 = DIRECTION ( 'NONE',  ( 0.000000000000000000, 0.000000000000000000, 1.000000000000000000 ) ) ;
#12568 = EDGE_CURVE ( 'NONE', #2066, #14471, #2566, .T. ) ;
#12569 = CARTESIAN_POINT ( 'NONE',  ( -54.99999999999996447, -14.99999999999998579, -10.00000000000000000 ) ) ;
#12570 = CARTESIAN_POINT ( 'NONE',  ( 44.05948171654945611, 48.20051614449764799, -4.345558710429044069 ) ) ;
#12571 = CARTESIAN_POINT ( 'NONE',  ( -1.000000000000000000, -6.008326913195983998, -0.8000000000000000444 ) ) ;
#12572 = FACE_OUTER_BOUND ( 'NONE', #13857, .T. ) ;
#12573 = ORIENTED_EDGE ( 'NONE', *, *, #3750, .F. ) ;
#12574 = DIRECTION ( 'NONE',  ( -1.000000000000000000, -1.040834085586084257E-16, -0.000000000000000000 ) ) ;
#12575 = CARTESIAN_POINT ( 'NONE',  ( 0.000000000000000000, 0.000000000000000000, 0.000000000000000000 ) ) ;
#12576 = CARTESIAN_POINT ( 'NONE',  ( 50.02271294988511841, 64.49948385550239038, 6.000000000000000888 ) ) ;
#12577 = DIRECTION ( 'NONE',  ( 0.000000000000000000, 0.000000000000000000, -1.000000000000000000 ) ) ;
#12578 = CARTESIAN_POINT ( 'NONE',  ( 47.74827507625478518, 46.59948385550239891, 7.007379884777227730 ) ) ;
#12579 = FACE_OUTER_BOUND ( 'NONE', #16662, .T. ) ;
#12580 = CARTESIAN_POINT ( 'NONE',  ( 45.27934281921082516, 61.70051614449766220, 6.458785618021089192 ) ) ;
#12581 = CARTESIAN_POINT ( 'NONE',  ( 55.11794222512599362, 60.80051614449766362, -3.688883143319583446 ) ) ;
#12582 = DIRECTION ( 'NONE',  ( -0.000000000000000000, -0.000000000000000000, -1.000000000000000000 ) ) ;
#12583 = PLANE ( 'NONE',  #11259 ) ;
#12584 = ORIENTED_EDGE ( 'NONE', *, *, #17114, .F. ) ;
#12585 = ORIENTED_EDGE ( 'NONE', *, *, #819, .F. ) ;
#12586 = PLANE ( 'NONE',  #8108 ) ;
#12587 = ORIENTED_EDGE ( 'NONE', *, *, #13461, .T. ) ;
#12588 = PLANE ( 'NONE',  #305 ) ;
#12589 = CIRCLE ( 'NONE', #3224, 20.00000000000000000 ) ;
#12590 = VERTEX_POINT ( 'NONE', #19033 ) ;
#12591 = DIRECTION ( 'NONE',  ( -1.000000000000000000, 0.000000000000000000, 0.000000000000000000 ) ) ;
#12592 = CARTESIAN_POINT ( 'NONE',  ( 52.29715082351547295, 54.39948385550239607, 6.992620115222774047 ) ) ;
#12593 = ORIENTED_EDGE ( 'NONE', *, *, #18903, .T. ) ;
#12594 = LINE ( 'NONE', #1931, #54 ) ;
#12595 = VERTEX_POINT ( 'NONE', #17359 ) ;
#12596 = CARTESIAN_POINT ( 'NONE',  ( 42.39856655714566358, 52.89948385550241028, 2.493737253992119207 ) ) ;
#12597 = DIRECTION ( 'NONE',  ( 1.000000000000000000, -0.000000000000000000, -0.000000000000000000 ) ) ;
#12598 = CARTESIAN_POINT ( 'NONE',  ( 44.05948171654949874, 62.79948385550241596, 4.345558710429105354 ) ) ;
#12599 = DIRECTION ( 'NONE',  ( 0.000000000000000000, 8.673617379884036458E-16, 1.000000000000000000 ) ) ;
#12600 = CARTESIAN_POINT ( 'NONE',  ( -10.93224627749298605, -36.74771600333134103, 0.000000000000000000 ) ) ;
#12601 = CARTESIAN_POINT ( 'NONE',  ( 50.02271294988505446, 60.50051614449765935, -7.000000000000000888 ) ) ;
#12602 = CARTESIAN_POINT ( 'NONE',  ( 55.08986747509849380, 45.20051614449766220, 3.727524721679155384 ) ) ;
#12603 = CARTESIAN_POINT ( 'NONE',  ( 42.63976443033212860, 56.99948385550241170, 0.02388180880522514787 ) ) ;
#12604 = LINE ( 'NONE', #845, #8792 ) ;
#12605 = CARTESIAN_POINT ( 'NONE',  ( 6.367873360227558344, -2.886751345948133984, -5.000000000000000000 ) ) ;
#12606 = ADVANCED_FACE ( 'NONE', ( #5575 ), #4113, .F. ) ;
#12607 = ORIENTED_EDGE ( 'NONE', *, *, #8658, .T. ) ;
#12608 = PRODUCT_DEFINITION_FORMATION_WITH_SPECIFIED_SOURCE ( 'ANY', '', #12728, .NOT_KNOWN. ) ;
#12609 = ORIENTED_EDGE ( 'NONE', *, *, #2592, .T. ) ;
#12610 = CARTESIAN_POINT ( 'NONE',  ( -10.75570504584937304, -36.18033988749900942, -9.000000000000000000 ) ) ;
#12611 =( NAMED_UNIT ( * ) SI_UNIT ( $, .STERADIAN. ) SOLID_ANGLE_UNIT ( ) );
#12612 = PRODUCT_RELATED_PRODUCT_CATEGORY ( 'part', '', ( #683 ) ) ;
#12613 = CARTESIAN_POINT ( 'NONE',  ( 49.97728705011488159, 53.49948385550240459, -7.000000000000000888 ) ) ;
#12614 = CARTESIAN_POINT ( 'NONE',  ( 1.925929944387235853E-31, 15.00000000000001599, 15.00000000000000000 ) ) ;
#12615 = VERTEX_POINT ( 'NONE', #4206 ) ;
#12616 = ORIENTED_EDGE ( 'NONE', *, *, #11076, .T. ) ;
#12617 = LINE ( 'NONE', #3808, #18052 ) ;
#12618 = EDGE_CURVE ( 'NONE', #15947, #4192, #3921, .T. ) ;
#12619 = EDGE_CURVE ( 'NONE', #3254, #11034, #7146, .T. ) ;
#12620 = ORIENTED_EDGE ( 'NONE', *, *, #8813, .T. ) ;
#12621 = CARTESIAN_POINT ( 'NONE',  ( 62.49999999999998579, 40.00000000000001421, 0.000000000000000000 ) ) ;
#12622 = VERTEX_POINT ( 'NONE', #14392 ) ;
#12623 = EDGE_CURVE ( 'NONE', #1343, #17671, #15877, .T. ) ;
#12624 = DIRECTION ( 'NONE',  ( 0.000000000000000000, 0.000000000000000000, -1.000000000000000000 ) ) ;
#12625 = CARTESIAN_POINT ( 'NONE',  ( -158.9999999999999716, -14.99999999999999645, -15.00000000000000000 ) ) ;
#12626 = EDGE_CURVE ( 'NONE', #5077, #15338, #3683, .T. ) ;
#12627 = CARTESIAN_POINT ( 'NONE',  ( 55.11794222512599362, 60.80051614449766362, -3.688883143319583446 ) ) ;
#12628 = DIRECTION ( 'NONE',  ( -0.000000000000000000, -0.000000000000000000, -1.000000000000000000 ) ) ;
#12629 = CARTESIAN_POINT ( 'NONE',  ( 17.32050807568866091, -9.999999999999797495, 9.000000000000000000 ) ) ;
#12630 = CARTESIAN_POINT ( 'NONE',  ( 4.000000000000003553, 0.000000000000000000, 0.000000000000000000 ) ) ;
#12631 = ADVANCED_FACE ( 'NONE', ( #980 ), #5773, .F. ) ;
#12632 = CARTESIAN_POINT ( 'NONE',  ( 41.58830220609386430, 58.00051614449765935, -0.02388180880514929535 ) ) ;
#12633 = EDGE_CURVE ( 'NONE', #17668, #12590, #13378, .T. ) ;
#12634 = ORIENTED_EDGE ( 'NONE', *, *, #9630, .T. ) ;
#12635 = ORIENTED_EDGE ( 'NONE', *, *, #18280, .F. ) ;
#12636 = DIRECTION ( 'NONE',  ( -0.000000000000000000, 0.000000000000000000, -1.000000000000000000 ) ) ;
#12637 =( NAMED_UNIT ( * ) SI_UNIT ( $, .STERADIAN. ) SOLID_ANGLE_UNIT ( ) );
#12638 = CONTEXT_DEPENDENT_SHAPE_REPRESENTATION ( #10655, #17619 ) ;
#12639 = ORIENTED_EDGE ( 'NONE', *, *, #3888, .F. ) ;
#12640 = DIRECTION ( 'NONE',  ( 0.000000000000000000, 0.000000000000000000, -1.000000000000000000 ) ) ;
#12641 = EDGE_CURVE ( 'NONE', #178, #4179, #4013, .T. ) ;
#12642 = CARTESIAN_POINT ( 'NONE',  ( 75.00000000000002842, -39.99999999999998579, 10.00000000000000000 ) ) ;
#12644 = EDGE_CURVE ( 'NONE', #12254, #2647, #16794, .T. ) ;
#12643 = ORIENTED_EDGE ( 'NONE', *, *, #12641, .F. ) ;
#12645 = CIRCLE ( 'NONE', #5129, 12.49999999999999645 ) ;
#12646 = EDGE_CURVE ( 'NONE', #11339, #2420, #8996, .T. ) ;
#12647 = CARTESIAN_POINT ( 'NONE',  ( 0.000000000000000000, 0.000000000000000000, -4.000000000000000000 ) ) ;
#12648 = DIRECTION ( 'NONE',  ( 0.000000000000000000, 0.000000000000000000, 1.000000000000000000 ) ) ;
#12649 = DIRECTION ( 'NONE',  ( -0.000000000000000000, -0.000000000000000000, -1.000000000000000000 ) ) ;
#12650 = AXIS2_PLACEMENT_3D ( 'NONE', #4197, #13304, #10164 ) ;
#12651 = CARTESIAN_POINT ( 'NONE',  ( 0.000000000000000000, 0.000000000000000000, -10.00000000000000000 ) ) ;
#12652 = CYLINDRICAL_SURFACE ( 'NONE', #14623, 2.649999999999988365 ) ;
#12653 = CARTESIAN_POINT ( 'NONE',  ( 56.65037692655918988, 61.89948385550241028, -2.184720259617163762 ) ) ;
#12654 = CARTESIAN_POINT ( 'NONE',  ( 0.000000000000000000, 0.4273491293402468805, -0.8000000000000000444 ) ) ;
#12655 = CARTESIAN_POINT ( 'NONE',  ( 42.39856655714566358, 58.89948385550241028, 2.493737253992119207 ) ) ;
#12656 = CARTESIAN_POINT ( 'NONE',  ( 44.05948171654945611, 58.20051614449764799, -4.345558710429044069 ) ) ;
#12657 = CARTESIAN_POINT ( 'NONE',  ( 19.89043790736544892, -17.90943073464672608, -9.000000000000000000 ) ) ;
#12658 = CARTESIAN_POINT ( 'NONE',  ( 6.095473853218515536, 4.853892138986921623, -1.592812200815479695 ) ) ;
#12659 = DIRECTION ( 'NONE',  ( -0.9768494444719831860, -0.2139279384156685671, 1.428280402131856228E-22 ) ) ;
#12660 =( REPRESENTATION_RELATIONSHIP ('NONE','NONE', #16703, #17450 ) REPRESENTATION_RELATIONSHIP_WITH_TRANSFORMATION ( #15879 )SHAPE_REPRESENTATION_RELATIONSHIP( ) );
#12661 = ORIENTED_EDGE ( 'NONE', *, *, #58, .T. ) ;
#12662 = VECTOR ( 'NONE', #594, 1000.000000000000000 ) ;
#12663 = DIRECTION ( 'NONE',  ( -1.000000000000000000, 0.000000000000000000, 0.000000000000000000 ) ) ;
#12664 = DIRECTION ( 'NONE',  ( 0.000000000000000000, 1.000000000000000000, 0.000000000000000000 ) ) ;
#12665 = CARTESIAN_POINT ( 'NONE',  ( 52.29715082351539479, 52.60051614449766078, -6.992620115222796251 ) ) ;
#12666 = CARTESIAN_POINT ( 'NONE',  ( 4.170895651974849905, -2.054890354522598273, 3.559174498016383748 ) ) ;
#12667 = CARTESIAN_POINT ( 'NONE',  ( 50.00000000000000000, 12.59655753109423237, 0.000000000000000000 ) ) ;
#12668 = VERTEX_POINT ( 'NONE', #419 ) ;
#12669 = CYLINDRICAL_SURFACE ( 'NONE', #15549, 5.000000000000007994 ) ;
#12670 = DIRECTION ( 'NONE',  ( 0.000000000000000000, 1.000000000000000000, 0.000000000000000000 ) ) ;
#12671 = EDGE_CURVE ( 'NONE', #11107, #9525, #13994, .T. ) ;
#12672 = DIRECTION ( 'NONE',  ( 0.000000000000000000, 0.000000000000000000, 1.000000000000000000 ) ) ;
#12673 = SURFACE_STYLE_FILL_AREA ( #2999 ) ;
#12674 = AXIS2_PLACEMENT_3D ( 'NONE', #9502, #4730, #6467 ) ;
#12675 = CYLINDRICAL_SURFACE ( 'NONE', #2956, 3.799999999999999378 ) ;
#12676 = CARTESIAN_POINT ( 'NONE',  ( 56.79116909180259398, 57.20051614449766220, 4.963592699178938972 ) ) ;
#12677 = ADVANCED_FACE ( 'NONE', ( #3360 ), #7951, .T. ) ;
#12678 = CARTESIAN_POINT ( 'NONE',  ( 43.69122665457040000, 60.00051614449765935, -0.02388180880515696977 ) ) ;
#12679 = CARTESIAN_POINT ( 'NONE',  ( 6.080745460913608902, 0.5192545390863916310, -1.000000000000000000 ) ) ;
#12680 = CARTESIAN_POINT ( 'NONE',  ( 6.095484975317565279, -1.047622383848427985, 4.999999999999999112 ) ) ;
#12681 = CIRCLE ( 'NONE', #18656, 9.999999999999998224 ) ;
#12682 = EDGE_LOOP ( 'NONE', ( #3629, #11881, #10914, #10759 ) ) ;
#12683 = VERTEX_POINT ( 'NONE', #5111 ) ;
#12684 = ORIENTED_EDGE ( 'NONE', *, *, #10222, .F. ) ;
#12685 = DIRECTION ( 'NONE',  ( -0.5000000000000016653, 0.8660254037844378194, 0.000000000000000000 ) ) ;
#12686 = ORIENTED_EDGE ( 'NONE', *, *, #16414, .F. ) ;
#12687 = CARTESIAN_POINT ( 'NONE',  ( -3.309651814758565180, -5.455921364805393026, 0.000000000000000000 ) ) ;
#12688 = EDGE_LOOP ( 'NONE', ( #10968, #10061, #16751, #2711, #11918, #11688 ) ) ;
#12689 = CARTESIAN_POINT ( 'NONE',  ( 0.5000000000000000000, -6.429618962271402616, -1.000000000000000000 ) ) ;
#12690 = CARTESIAN_POINT ( 'NONE',  ( 42.63976443033212149, 58.99948385550239038, 0.02388180880522514787 ) ) ;
#12691 = ORIENTED_EDGE ( 'NONE', *, *, #3794, .T. ) ;
#12692 = CARTESIAN_POINT ( 'NONE',  ( 6.403457969954082785, -2.888443235695457467, -5.002930439003169916 ) ) ;
#12693 = EDGE_LOOP ( 'NONE', ( #17143, #16423, #15089, #14275 ) ) ;
#12694 = CARTESIAN_POINT ( 'NONE',  ( 42.39856655714566358, 54.89948385550240317, 2.493737253992119207 ) ) ;
#12695 = DIRECTION ( 'NONE',  ( -1.000000000000000000, 0.000000000000000000, 1.224646799147353207E-16 ) ) ;
#12696 = CIRCLE ( 'NONE', #16773, 8.000000000000007105 ) ;
#12697 = CARTESIAN_POINT ( 'NONE',  ( 47.70284917648453415, 65.39948385550239607, -6.992620115222774047 ) ) ;
#12698 = CARTESIAN_POINT ( 'NONE',  ( 4.175075985190094485, 2.060370777630093464, -3.568666869285578080 ) ) ;
#12699 = DIRECTION ( 'NONE',  ( 0.8660254037844379305, 0.5000000000000013323, 0.000000000000000000 ) ) ;
#12700 = CARTESIAN_POINT ( 'NONE',  ( 44.03140696652198471, 59.80051614449766362, 4.306917132069485454 ) ) ;
#12701 = CARTESIAN_POINT ( 'NONE',  ( 56.30877334542961421, 61.99948385550241170, -0.02388180880520959434 ) ) ;
#12702 = AXIS2_PLACEMENT_3D ( 'NONE', #12432, #18439, #4986 ) ;
#12703 = CARTESIAN_POINT ( 'NONE',  ( 50.02271294988512551, 58.49948385550241170, 7.000000000000000888 ) ) ;
#12704 = FACE_OUTER_BOUND ( 'NONE', #9288, .T. ) ;
#12705 = DIRECTION ( 'NONE',  ( -0.04542589977017699732, 0.9989677110047501252, 0.000000000000000000 ) ) ;
#12706 = ORIENTED_EDGE ( 'NONE', *, *, #1416, .F. ) ;
#12707 = VERTEX_POINT ( 'NONE', #9602 ) ;
#12708 = DIRECTION ( 'NONE',  ( 0.1305261922200521840, -0.9914448613738103822, 0.000000000000000000 ) ) ;
#12709 =( NAMED_UNIT ( * ) PLANE_ANGLE_UNIT ( ) SI_UNIT ( $, .RADIAN. ) );
#12710 = CIRCLE ( 'NONE', #18991, 20.00000000000000000 ) ;
#12711 = CARTESIAN_POINT ( 'NONE',  ( 45.86712807150323812, 55.29948385550240175, -5.649768623646098220 ) ) ;
#12712 = DIRECTION ( 'NONE',  ( -1.000000000000000000, 0.000000000000000000, -0.000000000000000000 ) ) ;
#12713 = EDGE_LOOP ( 'NONE', ( #8206, #14888 ) ) ;
#12714 = EDGE_LOOP ( 'NONE', ( #4115, #4118 ) ) ;
#12715 = DIRECTION ( 'NONE',  ( 0.000000000000000000, 0.000000000000000000, -1.000000000000000000 ) ) ;
#12716 = CIRCLE ( 'NONE', #3637, 1.000000000000001110 ) ;
#12717 = ORIENTED_EDGE ( 'NONE', *, *, #7114, .F. ) ;
#12718 = CARTESIAN_POINT ( 'NONE',  ( 47.70284917648459810, 63.60051614449766078, 6.992620115222797139 ) ) ;
#12719 = VERTEX_POINT ( 'NONE', #18468 ) ;
#12720 = EDGE_CURVE ( 'NONE', #13559, #10976, #15577, .T. ) ;
#12721 = CARTESIAN_POINT ( 'NONE',  ( 56.66441430157296821, 46.09948385550240602, 2.141517661632100111 ) ) ;
#12722 = FACE_OUTER_BOUND ( 'NONE', #9660, .T. ) ;
#12723 = AXIS2_PLACEMENT_3D ( 'NONE', #11289, #14795, #10280 ) ;
#12724 = CARTESIAN_POINT ( 'NONE',  ( 50.02271294988506156, 60.50051614449766646, -6.000000000000000888 ) ) ;
#12725 = DIRECTION ( 'NONE',  ( -0.000000000000000000, -0.000000000000000000, 1.000000000000000000 ) ) ;
#12726 = DIRECTION ( 'NONE',  ( 1.000000000000000000, 0.000000000000000000, 0.000000000000000000 ) ) ;
#12727 = DIRECTION ( 'NONE',  ( -0.000000000000000000, -0.000000000000000000, 1.000000000000000000 ) ) ;
#12728 = PRODUCT ( 'hex flange bolt small_iso_ISO 4162 - M8 x 45 x 22-N', 'hex flange bolt small_iso_ISO 4162 - M8 x 45 x 22-N', '', ( #490 ) ) ;
#12729 = EDGE_LOOP ( 'NONE', ( #2914, #7584 ) ) ;
#12730 = ORIENTED_EDGE ( 'NONE', *, *, #19015, .F. ) ;
#12731 = CARTESIAN_POINT ( 'NONE',  ( 4.000000000000000000, -1.700175430507292473, -3.320327275037661785 ) ) ;
#12732 = PRESENTATION_STYLE_ASSIGNMENT (( #3530 ) ) ;
#12733 = VECTOR ( 'NONE', #2801, 1000.000000000000000 ) ;
#12734 = ADVANCED_FACE ( 'NONE', ( #18571 ), #13741, .T. ) ;
#12735 = EDGE_LOOP ( 'NONE', ( #14977, #7629, #11572, #8642, #16999, #18766 ) ) ;
#12736 = AXIS2_PLACEMENT_3D ( 'NONE', #6263, #1863, #4803 ) ;
#12737 = DIRECTION ( 'NONE',  ( 0.000000000000000000, 0.000000000000000000, 1.000000000000000000 ) ) ;
#12738 = CARTESIAN_POINT ( 'NONE',  ( 62.49999999999998579, 45.00000000000001421, -5.000000000000000000 ) ) ;
#12739 = ORIENTED_EDGE ( 'NONE', *, *, #4498, .T. ) ;
#12740 = EDGE_CURVE ( 'NONE', #10144, #4604, #3741, .T. ) ;
#12741 = CLOSED_SHELL ( 'NONE', ( #12606, #2227, #18814, #15202, #7856, #17975, #3288, #5920, #18056, #2705, #16700, #13630, #4056, #4611, #17673, #19055, #15866, #4296, #12502, #411, #13861, #1300, #13224, #6454, #12008, #8609, #9676, #192, #8322, #4742, #17181, #16958, #12864, #14060, #17656, #14551, #8130, #707, #8917, #8186, #15429, #224, #14170, #10400, #7711, #15441, #13826, #9975, #15998 ) ) ;
#12742 = CARTESIAN_POINT ( 'NONE',  ( 0.000000000000000000, 0.5192545390863916310, -1.000000000000000000 ) ) ;
#12743 = CARTESIAN_POINT ( 'NONE',  ( 62.50000000000000000, 20.00000000000001421, 9.999999999999998224 ) ) ;
#12744 = ADVANCED_FACE ( 'NONE', ( #4919 ), #13394, .T. ) ;
#12745 = CARTESIAN_POINT ( 'NONE',  ( 4.170895651974850793, 4.109780709045216085, 3.964526709274768569E-16 ) ) ;
#12746 = DIRECTION ( 'NONE',  ( 1.000000000000000000, 0.000000000000000000, 0.000000000000000000 ) ) ;
#12747 = ADVANCED_FACE ( 'NONE', ( #6577 ), #17087, .F. ) ;
#12748 = CIRCLE ( 'NONE', #8360, 8.000000000000007105 ) ;
#12749 = CARTESIAN_POINT ( 'NONE',  ( 10.00000000000000000, 0.000000000000000000, -9.999999999999998224 ) ) ;
#12750 = CARTESIAN_POINT ( 'NONE',  ( 44.91013252490152752, 46.79948385550240886, 3.727524721679198461 ) ) ;
#12751 = DIRECTION ( 'NONE',  ( -0.000000000000000000, -1.000000000000000000, -0.000000000000000000 ) ) ;
#12752 = CARTESIAN_POINT ( 'NONE',  ( 57.61547081786812896, 64.09948385550239891, 2.450534656007040901 ) ) ;
#12753 = CARTESIAN_POINT ( 'NONE',  ( 56.66441430157294690, 58.90051614449766504, -2.141517661632166281 ) ) ;
#12754 = EDGE_CURVE ( 'NONE', #9304, #153, #603, .T. ) ;
#12755 = DIRECTION ( 'NONE',  ( 1.000000000000000000, 0.000000000000000000, 0.000000000000000000 ) ) ;
#12756 = DIRECTION ( 'NONE',  ( 0.000000000000000000, 0.000000000000000000, 1.000000000000000000 ) ) ;
#12757 = DIRECTION ( 'NONE',  ( 0.000000000000000000, 0.000000000000000000, -1.000000000000000000 ) ) ;
#12758 = AXIS2_PLACEMENT_3D ( 'NONE', #5196, #3355, #7857 ) ;
#12759 = ORIENTED_EDGE ( 'NONE', *, *, #2604, .F. ) ;
#12760 = CARTESIAN_POINT ( 'NONE',  ( 0.000000000000000000, -1.773042676681341856, 2.276824562219559311E-15 ) ) ;
#12761 = DIRECTION ( 'NONE',  ( 1.000000000000000000, 0.000000000000000000, 0.000000000000000000 ) ) ;
#12762 = COLOUR_RGB ( '',1.000000000000000000, 0.9490196078431372140, 0.9098039215686274384 ) ;
#12763 = CARTESIAN_POINT ( 'NONE',  ( 50.02271294988505446, 50.50051614449765935, -7.000000000000000888 ) ) ;
#12764 = ADVANCED_FACE ( 'NONE', ( #16896 ), #17179, .F. ) ;
#12765 = DIRECTION ( 'NONE',  ( 0.000000000000000000, 0.000000000000000000, 1.000000000000000000 ) ) ;
#12766 = ADVANCED_FACE ( 'NONE', ( #15409, #1989 ), #6303, .F. ) ;
#12767 = CARTESIAN_POINT ( 'NONE',  ( 4.197393957002303999, -0.4069871074557456780, -3.503767560748925813 ) ) ;
#12768 = VERTEX_POINT ( 'NONE', #4829 ) ;
#12769 = DIRECTION ( 'NONE',  ( -0.7779254092217071648, -0.6283566325640553840, 0.000000000000000000 ) ) ;
#12770 = CARTESIAN_POINT ( 'NONE',  ( -154.9999999999999716, -14.99999999999999645, 3.999999999999999112 ) ) ;
#12771 = DIRECTION ( 'NONE',  ( -0.000000000000000000, -0.000000000000000000, -1.000000000000000000 ) ) ;
#12772 = CARTESIAN_POINT ( 'NONE',  ( 56.66441430157296821, 48.09948385550240602, 2.141517661632100111 ) ) ;
#12773 = FACE_OUTER_BOUND ( 'NONE', #9736, .T. ) ;
#12774 = VECTOR ( 'NONE', #432, 1000.000000000000000 ) ;
#12775 = CARTESIAN_POINT ( 'NONE',  ( 58.41169779390614281, 47.99948385550239038, -0.02388180880523160798 ) ) ;
#12776 = CARTESIAN_POINT ( 'NONE',  ( 44.30067958973594955, 64.10051614449766078, -1.875703265242155693 ) ) ;
#12777 = CIRCLE ( 'NONE', #13410, 20.00000000000000000 ) ;
#12778 = FACE_OUTER_BOUND ( 'NONE', #13514, .T. ) ;
#12779 = FACE_BOUND ( 'NONE', #14448, .T. ) ;
#12780 = ORIENTED_EDGE ( 'NONE', *, *, #15267, .T. ) ;
#12781 = EDGE_LOOP ( 'NONE', ( #12031, #14342, #5522, #14318 ) ) ;
#12782 =( GEOMETRIC_REPRESENTATION_CONTEXT ( 3 ) GLOBAL_UNCERTAINTY_ASSIGNED_CONTEXT ( ( #1672 ) ) GLOBAL_UNIT_ASSIGNED_CONTEXT ( ( #16777, #15197, #13818 ) ) REPRESENTATION_CONTEXT ( 'NONE', 'WORKASPACE' ) );
#12783 = ORIENTED_EDGE ( 'NONE', *, *, #18774, .F. ) ;
#12784 = CARTESIAN_POINT ( 'NONE',  ( -150.9999999999999716, -14.99999999999999645, -15.00000000000000000 ) ) ;
#12785 = ORIENTED_EDGE ( 'NONE', *, *, #11351, .F. ) ;
#12786 = DIRECTION ( 'NONE',  ( 0.000000000000000000, -0.000000000000000000, 1.000000000000000000 ) ) ;
#12787 = ORIENTED_EDGE ( 'NONE', *, *, #3750, .T. ) ;
#12788 = DIRECTION ( 'NONE',  ( -0.000000000000000000, 0.000000000000000000, -1.000000000000000000 ) ) ;
#12789 = AXIS2_PLACEMENT_3D ( 'NONE', #14883, #16174, #13417 ) ;
#12790 = EDGE_CURVE ( 'NONE', #13890, #9546, #15904, .T. ) ;
#12791 = CARTESIAN_POINT ( 'NONE',  ( 54.09612160359786515, 55.69948385550240744, -5.676469297603166098 ) ) ;
#12792 = CIRCLE ( 'NONE', #4342, 0.9999999999999995559 ) ;
#12793 = ORIENTED_EDGE ( 'NONE', *, *, #10774, .T. ) ;
#12794 = ADVANCED_FACE ( 'NONE', ( #6477 ), #15314, .F. ) ;
#12795 = DIRECTION ( 'NONE',  ( -0.000000000000000000, -0.000000000000000000, 1.000000000000000000 ) ) ;
#12796 = VERTEX_POINT ( 'NONE', #18954 ) ;
#12797 = CARTESIAN_POINT ( 'NONE',  ( 54.72065718078924590, 50.29948385550240886, 6.458785618021043895 ) ) ;
#12798 = CARTESIAN_POINT ( 'NONE',  ( 3.958476099524539382, -1.406653531810738933, -3.499999999999999556 ) ) ;
#12799 = CARTESIAN_POINT ( 'NONE',  ( 50.02271294988511841, 48.49948385550241170, 6.000000000000000888 ) ) ;
#12800 = EDGE_CURVE ( 'NONE', #16565, #164, #3939, .T. ) ;
#12801 = CARTESIAN_POINT ( 'NONE',  ( 4.052424581287595196, 3.786734753434853662, 0.5771415817955924954 ) ) ;
#12802 = DIRECTION ( 'NONE',  ( 0.02857142857142857054, 0.9995917534020515305, 0.000000000000000000 ) ) ;
#12803 = CARTESIAN_POINT ( 'NONE',  ( 55.96859303347802239, 62.80051614449766362, -4.306917132069484566 ) ) ;
#12804 = CARTESIAN_POINT ( 'NONE',  ( 46.49166364869460466, 62.69948385550240744, 4.867452303228209765 ) ) ;
#12805 = DIRECTION ( 'NONE',  ( 1.000000000000000000, 0.000000000000000000, 0.000000000000000000 ) ) ;
#12806 = DIRECTION ( 'NONE',  ( -0.000000000000000000, -0.000000000000000000, 1.000000000000000000 ) ) ;
#12807 = ORIENTED_EDGE ( 'NONE', *, *, #16972, .T. ) ;
#12808 = EDGE_LOOP ( 'NONE', ( #18534, #2494, #5855, #7886, #732 ) ) ;
#12809 = CARTESIAN_POINT ( 'NONE',  ( 2.000000000000000000, 0.000000000000000000, 0.000000000000000000 ) ) ;
#12810 = ORIENTED_EDGE ( 'NONE', *, *, #176, .T. ) ;
#12811 = ADVANCED_FACE ( 'NONE', ( #1193 ), #14006, .T. ) ;
#12812 = CARTESIAN_POINT ( 'NONE',  ( 52.25172492374522903, 61.59948385550239891, -7.007379884777225953 ) ) ;
#12813 = CARTESIAN_POINT ( 'NONE',  ( 0.000000000000000000, 4.898587196589412829E-16, -4.000000000000000000 ) ) ;
#12814 =( GEOMETRIC_REPRESENTATION_CONTEXT ( 3 ) GLOBAL_UNCERTAINTY_ASSIGNED_CONTEXT ( ( #16573 ) ) GLOBAL_UNIT_ASSIGNED_CONTEXT ( ( #7576, #37, #13558 ) ) REPRESENTATION_CONTEXT ( 'NONE', 'WORKASPACE' ) );
#12815 = EDGE_LOOP ( 'NONE', ( #4989, #7224, #5366, #4555 ) ) ;
#12816 = ORIENTED_EDGE ( 'NONE', *, *, #2351, .F. ) ;
#12817 = DIRECTION ( 'NONE',  ( 1.000000000000000000, 0.000000000000000000, 0.000000000000000000 ) ) ;
#12818 = ADVANCED_FACE ( 'NONE', ( #15898 ), #17282, .F. ) ;
#12819 = VERTEX_POINT ( 'NONE', #9705 ) ;
#12820 = CARTESIAN_POINT ( 'NONE',  ( 7.336184427528458230, 9.926022037524705097E-16, 8.105212085995399107 ) ) ;
#12821 = ORIENTED_EDGE ( 'NONE', *, *, #6626, .T. ) ;
#12822 = CIRCLE ( 'NONE', #4371, 3.500000000000000000 ) ;
#12823 = VECTOR ( 'NONE', #8684, 1000.000000000000000 ) ;
#12824 = CARTESIAN_POINT ( 'NONE',  ( 47.70284917648453415, 51.39948385550238896, -6.992620115222774047 ) ) ;
#12825 = PLANE ( 'NONE',  #1791 ) ;
#12826 = CARTESIAN_POINT ( 'NONE',  ( 48.07319477248762496, 60.40051614449765793, -6.007379884777208190 ) ) ;
#12827 = CARTESIAN_POINT ( 'NONE',  ( 0.000000000000000000, 0.000000000000000000, -1.000000000000000000 ) ) ;
#12828 = FACE_OUTER_BOUND ( 'NONE', #17249, .T. ) ;
#12829 = VECTOR ( 'NONE', #15997, 1000.000000000000000 ) ;
#12830 = FACE_BOUND ( 'NONE', #10146, .T. ) ;
#12831 = VERTEX_POINT ( 'NONE', #11371 ) ;
#12832 = ORIENTED_EDGE ( 'NONE', *, *, #11299, .F. ) ;
#12833 = CARTESIAN_POINT ( 'NONE',  ( 4.000000000000000000, 2.512223110932545023, -3.469391141908803711 ) ) ;
#12834 = DIRECTION ( 'NONE',  ( 0.000000000000000000, 0.000000000000000000, 1.000000000000000000 ) ) ;
#12835 = VERTEX_POINT ( 'NONE', #1094 ) ;
#12836 = CARTESIAN_POINT ( 'NONE',  ( 4.000000000000000000, 2.309401076758515803, -0.4999999999999995559 ) ) ;
#12837 = AXIS2_PLACEMENT_3D ( 'NONE', #12099, #6039, #18107 ) ;
#12838 = ORIENTED_EDGE ( 'NONE', *, *, #13722, .T. ) ;
#12839 = DIRECTION ( 'NONE',  ( 0.000000000000000000, 0.000000000000000000, 1.000000000000000000 ) ) ;
#12840 = CARTESIAN_POINT ( 'NONE',  ( 4.114405500665256454, 4.051151509359430136, -5.737475420082528345E-17 ) ) ;
#12841 = AXIS2_PLACEMENT_3D ( 'NONE', #1591, #117, #16691 ) ;
#12842 = FACE_OUTER_BOUND ( 'NONE', #8399, .T. ) ;
#12843 = CARTESIAN_POINT ( 'NONE',  ( 0.03027795055833727364, 0.6888063905328611902, 3.500000000000000888 ) ) ;
#12844 = CARTESIAN_POINT ( 'NONE',  ( 53.50833635130540955, 49.69948385550240744, -4.867452303228209765 ) ) ;
#12845 = AXIS2_PLACEMENT_3D ( 'NONE', #2840, #11934, #17649 ) ;
#12846 = DIRECTION ( 'NONE',  ( 0.000000000000000000, 0.000000000000000000, 1.000000000000000000 ) ) ;
#12847 = AXIS2_PLACEMENT_3D ( 'NONE', #7892, #3675, #9639 ) ;
#12848 = CARTESIAN_POINT ( 'NONE',  ( 55.96859303347804371, 48.19948385550240033, 4.306917132069425946 ) ) ;
#12849 = CARTESIAN_POINT ( 'NONE',  ( 45.31609314410960820, 50.30051614449766362, -6.485486291978072693 ) ) ;
#12850 = CIRCLE ( 'NONE', #9405, 6.080745460913608902 ) ;
#12851 = CARTESIAN_POINT ( 'NONE',  ( 1.000000000000000000, -5.408326913195983465, -0.8000000000000000444 ) ) ;
#12852 = LINE ( 'NONE', #604, #15056 ) ;
#12853 = ADVANCED_FACE ( 'NONE', ( #14314 ), #255, .T. ) ;
#12854 = CARTESIAN_POINT ( 'NONE',  ( 0.000000000000000000, 0.000000000000000000, 0.000000000000000000 ) ) ;
#12855 = EDGE_LOOP ( 'NONE', ( #17332, #16961, #8945, #13727 ) ) ;
#12856 = VECTOR ( 'NONE', #9694, 1000.000000000000000 ) ;
#12857 = SURFACE_STYLE_FILL_AREA ( #6582 ) ;
#12858 = EDGE_CURVE ( 'NONE', #6513, #3553, #10000, .T. ) ;
#12859 = LINE ( 'NONE', #11181, #12501 ) ;
#12860 = AXIS2_PLACEMENT_3D ( 'NONE', #15845, #2534, #7014 ) ;
#12861 = VECTOR ( 'NONE', #12582, 1000.000000000000000 ) ;
#12862 = CARTESIAN_POINT ( 'NONE',  ( 49.97728705011495265, 55.50051614449766646, 7.000000000000000888 ) ) ;
#12863 = EDGE_CURVE ( 'NONE', #13093, #7769, #6204, .T. ) ;
#12864 = ADVANCED_FACE ( 'NONE', ( #6864 ), #11568, .F. ) ;
#12865 = DIRECTION ( 'NONE',  ( 1.000000000000000000, 0.000000000000000000, 0.000000000000000000 ) ) ;
#12866 = CARTESIAN_POINT ( 'NONE',  ( -19.02113032590304442, -26.18033988749903074, -9.000000000000000000 ) ) ;
#12867 = ORIENTED_EDGE ( 'NONE', *, *, #16885, .F. ) ;
#12868 = CARTESIAN_POINT ( 'NONE',  ( 0.000000000000000000, -3.031088913245531202, 1.750000000000006439 ) ) ;
#12869 = CARTESIAN_POINT ( 'NONE',  ( -62.49999999999997158, 45.00000000000001421, 15.00000000000000000 ) ) ;
#12870 = EDGE_CURVE ( 'NONE', #5817, #9490, #2587, .T. ) ;
#12871 = FACE_OUTER_BOUND ( 'NONE', #13946, .T. ) ;
#12872 = CARTESIAN_POINT ( 'NONE',  ( 56.66441430157296821, 54.09948385550240602, 2.141517661632100111 ) ) ;
#12873 = CARTESIAN_POINT ( 'NONE',  ( -162.9999999999999716, -14.99999999999999645, 15.00000000000000000 ) ) ;
#12874 = CARTESIAN_POINT ( 'NONE',  ( 47.42335538002188144, 48.59948385550239891, 8.007379884777233059 ) ) ;
#12875 =( NAMED_UNIT ( * ) PLANE_ANGLE_UNIT ( ) SI_UNIT ( $, .RADIAN. ) );
#12876 = CARTESIAN_POINT ( 'NONE',  ( 54.13287192849671214, 44.70051614449766220, -5.649768623646139964 ) ) ;
#12877 = DIRECTION ( 'NONE',  ( 0.000000000000000000, 1.000000000000000000, 0.000000000000000000 ) ) ;
#12878 = AXIS2_PLACEMENT_3D ( 'NONE', #9075, #6140, #10444 ) ;
#12879 = CARTESIAN_POINT ( 'NONE',  ( 2.899426713160750069, -23.82535289025860337, -8.999999999999996447 ) ) ;
#12880 = AXIS2_PLACEMENT_3D ( 'NONE', #7262, #18055, #7452 ) ;
#12882 = ORIENTED_EDGE ( 'NONE', *, *, #17437, .F. ) ;
#12881 = EDGE_CURVE ( 'NONE', #8876, #9761, #5299, .T. ) ;
#12883 = EDGE_CURVE ( 'NONE', #18188, #5237, #13084, .T. ) ;
#12884 = ORIENTED_EDGE ( 'NONE', *, *, #2087, .T. ) ;
#12885 = CARTESIAN_POINT ( 'NONE',  ( 20.00000000000000000, -14.99999999999999289, -23.00000000000000000 ) ) ;
#12886 = ORIENTED_EDGE ( 'NONE', *, *, #17545, .T. ) ;
#12887 = PLANE ( 'NONE',  #16276 ) ;
#12888 = VERTEX_POINT ( 'NONE', #13145 ) ;
#12889 = DIRECTION ( 'NONE',  ( 1.000000000000000000, 0.000000000000000000, -0.000000000000000000 ) ) ;
#12891 = B_SPLINE_CURVE_WITH_KNOTS ( 'NONE', 3,
 ( #1849, #13796, #18332, #7023 ),
 .UNSPECIFIED., .F., .F.,
 ( 4, 4 ),
 ( 0.002080789711329271950, 0.004173039763574510827 ),
 .UNSPECIFIED. ) ;
#12890 = CARTESIAN_POINT ( 'NONE',  ( 43.33558569842703179, 57.09948385550240602, -2.141517661632099223 ) ) ;
#12892 = VERTEX_POINT ( 'NONE', #7165 ) ;
#12893 = LINE ( 'NONE', #1223, #7424 ) ;
#12894 = ORIENTED_EDGE ( 'NONE', *, *, #14771, .T. ) ;
#12895 = CARTESIAN_POINT ( 'NONE',  ( 52.62207051974839089, 62.39948385550240317, 7.992620115222770494 ) ) ;
#12896 = CARTESIAN_POINT ( 'NONE',  ( 3.680118525130245732, -2.494084732383344605, -0.3507732604232533524 ) ) ;
#12897 = CARTESIAN_POINT ( 'NONE',  ( 46.49166364869460466, 52.69948385550240744, 4.867452303228209765 ) ) ;
#12898 = DIRECTION ( 'NONE',  ( -0.000000000000000000, 0.000000000000000000, 1.000000000000000000 ) ) ;
#12899 = CIRCLE ( 'NONE', #11958, 4.000000000000003553 ) ;
#12900 = DIRECTION ( 'NONE',  ( 1.000000000000000000, 0.000000000000000000, 0.000000000000000000 ) ) ;
#12901 = CARTESIAN_POINT ( 'NONE',  ( 47.42335538002180328, 46.40051614449765793, -8.007379884777206414 ) ) ;
#12902 = CARTESIAN_POINT ( 'NONE',  ( 43.69122665457040000, 60.99948385550241170, 0.02388180880521036456 ) ) ;
#12903 = DIRECTION ( 'NONE',  ( -0.5000000000000041078, 0.8660254037844362651, 0.000000000000000000 ) ) ;
#12904 = LINE ( 'NONE', #14363, #10956 ) ;
#12905 = VERTEX_POINT ( 'NONE', #894 ) ;
#12906 = ORIENTED_EDGE ( 'NONE', *, *, #13386, .T. ) ;
#12907 = DIRECTION ( 'NONE',  ( 0.000000000000000000, -1.000000000000000000, 9.783878858594328898E-16 ) ) ;
#12908 = VERTEX_POINT ( 'NONE', #19053 ) ;
#12909 = CARTESIAN_POINT ( 'NONE',  ( 43.34962307344081012, 56.89948385550240317, 2.184720259617164650 ) ) ;
#12910 = CARTESIAN_POINT ( 'NONE',  ( 0.000000000000000000, 5.773502691896261751, -2.749426538070115714E-16 ) ) ;
#12911 = ORIENTED_EDGE ( 'NONE', *, *, #14173, .F. ) ;
#12912 = EDGE_LOOP ( 'NONE', ( #2830, #11710, #3437, #17134, #17636, #6188, #18709, #7124, #7387, #2922 ) ) ;
#12913 = DIRECTION ( 'NONE',  ( 0.000000000000000000, 0.000000000000000000, 1.000000000000000000 ) ) ;
#12914 = EDGE_LOOP ( 'NONE', ( #1420, #4185, #13658, #17271 ) ) ;
#12915 = DIRECTION ( 'NONE',  ( 0.000000000000000000, -0.000000000000000000, -1.000000000000000000 ) ) ;
#12916 = ORIENTED_EDGE ( 'NONE', *, *, #3413, .T. ) ;
#12917 = CARTESIAN_POINT ( 'NONE',  ( 45.90387839640214196, 52.69948385550240033, 5.676469297603166098 ) ) ;
#12918 = DIRECTION ( 'NONE',  ( 0.000000000000000000, 0.000000000000000000, 1.000000000000000000 ) ) ;
#12919 = AXIS2_PLACEMENT_3D ( 'NONE', #5533, #3883, #8767 ) ;
#12920 = CARTESIAN_POINT ( 'NONE',  ( 56.66441430157294690, 44.90051614449765793, -2.141517661632166281 ) ) ;
#12921 = CARTESIAN_POINT ( 'NONE',  ( 6.534838248920899595, 5.903531555104835071, 8.098083288904839678E-18 ) ) ;
#12922 = ADVANCED_FACE ( 'NONE', ( #5596 ), #17582, .F. ) ;
#12923 = PLANE ( 'NONE',  #12388 ) ;
#12924 = AXIS2_PLACEMENT_3D ( 'NONE', #3063, #19356, #10294 ) ;
#12925 = DIRECTION ( 'NONE',  ( 0.9781476007338055778, 0.2079116908177597867, 0.000000000000000000 ) ) ;
#12926 = EDGE_CURVE ( 'NONE', #5570, #8337, #7768, .T. ) ;
#12927 = ORIENTED_EDGE ( 'NONE', *, *, #5195, .T. ) ;
#12928 = ORIENTED_EDGE ( 'NONE', *, *, #8437, .F. ) ;
#12929 = CARTESIAN_POINT ( 'NONE',  ( 3.972709601346592123, 3.429395227388311262, 1.191688283765307332 ) ) ;
#12930 = CARTESIAN_POINT ( 'NONE',  ( -19.89043790736547379, -17.90943073464699609, -9.000000000000000000 ) ) ;
#12931 = DIRECTION ( 'NONE',  ( 1.734723475976806848E-16, 1.000000000000000000, 0.000000000000000000 ) ) ;
#12932 = ORIENTED_EDGE ( 'NONE', *, *, #9990, .T. ) ;
#12933 = CARTESIAN_POINT ( 'NONE',  ( 6.367873360227558344, 5.773502691896261751, 0.000000000000000000 ) ) ;
#12934 = ORIENTED_EDGE ( 'NONE', *, *, #15447, .T. ) ;
#12935 = EDGE_LOOP ( 'NONE', ( #15347, #4602, #11430, #2445 ) ) ;
#12936 = DIRECTION ( 'NONE',  ( 1.000000000000000000, 0.000000000000000000, 0.000000000000000000 ) ) ;
#12937 = DIRECTION ( 'NONE',  ( 0.000000000000000000, 0.000000000000000000, -1.000000000000000000 ) ) ;
#12938 = CARTESIAN_POINT ( 'NONE',  ( 55.11794222512599362, 50.80051614449766362, -3.688883143319583446 ) ) ;
#12939 = DIRECTION ( 'NONE',  ( 0.000000000000000000, 0.000000000000000000, -1.000000000000000000 ) ) ;
#12940 = DIRECTION ( 'NONE',  ( -1.000000000000000000, 0.000000000000000000, 0.000000000000000000 ) ) ;
#12941 = CARTESIAN_POINT ( 'NONE',  ( 51.92680522751233951, 51.59948385550240602, -6.007379884777223289 ) ) ;
#12942 = CARTESIAN_POINT ( 'NONE',  ( 0.000000000000000000, -1.773042676681341856, 2.276824562219559311E-15 ) ) ;
#12943 = CARTESIAN_POINT ( 'NONE',  ( 49.97728705011486738, 63.49948385550241170, -8.000000000000001776 ) ) ;
#12944 = CARTESIAN_POINT ( 'NONE',  ( 54.72065718078918906, 48.70051614449766930, -6.458785618021089192 ) ) ;
#12945 = CARTESIAN_POINT ( 'NONE',  ( -1.000000000000000000, -14.00000000000000000, 8.999999999999998224 ) ) ;
#12946 = CARTESIAN_POINT ( 'NONE',  ( -154.9999999999999716, -14.99999999999999645, 17.00000000000000000 ) ) ;
#12947 = DIRECTION ( 'NONE',  ( 0.5135024480563477045, 0.000000000000000000, 0.8580881282479897454 ) ) ;
#12948 = ORIENTED_EDGE ( 'NONE', *, *, #16013, .F. ) ;
#12949 = DIRECTION ( 'NONE',  ( -0.9768494444668812671, -0.2139279384389642935, 0.000000000000000000 ) ) ;
#12950 = VECTOR ( 'NONE', #18606, 1000.000000000000000 ) ;
#12951 = FACE_OUTER_BOUND ( 'NONE', #2221, .T. ) ;
#12952 = CARTESIAN_POINT ( 'NONE',  ( 43.33558569842706021, 49.90051614449766504, 2.141517661632167169 ) ) ;
#12953 = AXIS2_PLACEMENT_3D ( 'NONE', #14620, #1206, #18970 ) ;
#12954 = CYLINDRICAL_SURFACE ( 'NONE', #17855, 20.00000000000000000 ) ;
#12955 = DIRECTION ( 'NONE',  ( -1.000000000000000000, 0.000000000000000000, 0.000000000000000000 ) ) ;
#12956 = ORIENTED_EDGE ( 'NONE', *, *, #6503, .F. ) ;
#12957 = DIRECTION ( 'NONE',  ( 0.000000000000000000, -0.5000000000000011102, -0.8660254037844379305 ) ) ;
#12958 = EDGE_CURVE ( 'NONE', #11651, #488, #8063, .T. ) ;
#12959 = CARTESIAN_POINT ( 'NONE',  ( 0.5636800770130377947, 4.293361309317166530, -3.531542292954102713 ) ) ;
#12960 = CARTESIAN_POINT ( 'NONE',  ( 52.29715082351547295, 50.39948385550240317, 6.992620115222774047 ) ) ;
#12961 = CARTESIAN_POINT ( 'NONE',  ( -154.9999999999999716, -14.99999999999999645, 9.000000000000000000 ) ) ;
#12962 = CARTESIAN_POINT ( 'NONE',  ( 43.18075615816994173, 63.80051614449766362, 4.924951120819380357 ) ) ;
#12963 = CARTESIAN_POINT ( 'NONE',  ( 2.449293598294706513E-15, -20.00000000000000000, 9.000000000000000000 ) ) ;
#12964 = CARTESIAN_POINT ( 'NONE',  ( 52.29715082351538769, 46.60051614449766078, -6.992620115222796251 ) ) ;
#12965 = VECTOR ( 'NONE', #14617, 1000.000000000000000 ) ;
#12966 = CARTESIAN_POINT ( 'NONE',  ( 5.000000000000003553, -20.00000000000000000, -8.999999999999998224 ) ) ;
#12967 = CARTESIAN_POINT ( 'NONE',  ( 6.092439126518621073, 1.005559546149547678, 4.999999999999999112 ) ) ;
#12968 = CIRCLE ( 'NONE', #5145, 2.149999999999999023 ) ;
#12969 = ORIENTED_EDGE ( 'NONE', *, *, #7876, .T. ) ;
#12970 = EDGE_LOOP ( 'NONE', ( #18682, #11113, #15538 ) ) ;
#12971 = DIRECTION ( 'NONE',  ( -1.000000000000000000, -0.000000000000000000, -0.000000000000000000 ) ) ;
#12972 = ORIENTED_EDGE ( 'NONE', *, *, #2201, .T. ) ;
#12973 = CARTESIAN_POINT ( 'NONE',  ( -30.00000000000000000, 3.000000000000002665, -5.999999999999998224 ) ) ;
#12974 = EDGE_CURVE ( 'NONE', #15388, #1761, #9939, .T. ) ;
#12975 = ORIENTED_EDGE ( 'NONE', *, *, #11907, .T. ) ;
#12976 = CARTESIAN_POINT ( 'NONE',  ( 4.024499207728657879, 2.323545700935571556, -3.572172305156506411 ) ) ;
#12977 = CARTESIAN_POINT ( 'NONE',  ( 54.09612160359786515, 59.69948385550240033, -5.676469297603166098 ) ) ;
#12978 = EDGE_LOOP ( 'NONE', ( #18306, #16778, #1253, #19214 ) ) ;
#12979 = CARTESIAN_POINT ( 'NONE',  ( 1.753358200816401209E-16, -0.4883827417527520920, -4.999999999999999112 ) ) ;
#12980 = ORIENTED_EDGE ( 'NONE', *, *, #4485, .T. ) ;
#12981 = CARTESIAN_POINT ( 'NONE',  ( 52.62207051974839089, 60.39948385550241028, 7.992620115222770494 ) ) ;
#12982 = AXIS2_PLACEMENT_3D ( 'NONE', #15099, #13430, #10181 ) ;
#12983 = LINE ( 'NONE', #5529, #19243 ) ;
#12984 = EDGE_CURVE ( 'NONE', #10775, #16015, #800, .T. ) ;
#12985 = CARTESIAN_POINT ( 'NONE',  ( 44.30067958973596376, 48.89948385550241028, 1.875703265242204099 ) ) ;
#12986 = DIRECTION ( 'NONE',  ( 0.000000000000000000, -0.5000000000000011102, -0.8660254037844379305 ) ) ;
#12987 = EDGE_CURVE ( 'NONE', #8359, #4627, #16852, .T. ) ;
#12988 = DIRECTION ( 'NONE',  ( -1.000000000000000000, 0.000000000000000000, 0.000000000000000000 ) ) ;
#12989 = CARTESIAN_POINT ( 'NONE',  ( 43.18075615816994173, 49.80051614449765651, 4.924951120819380357 ) ) ;
#12990 = VECTOR ( 'NONE', #8783, 1000.000000000000000 ) ;
#12991 = CARTESIAN_POINT ( 'NONE',  ( 55.69932041026405045, 49.10051614449766788, 1.875703265242156359 ) ) ;
#12992 = CARTESIAN_POINT ( 'NONE',  ( -17.32050807568872841, -30.00000000000008171, 9.000000000000000000 ) ) ;
#12993 = CARTESIAN_POINT ( 'NONE',  ( 6.367873360227558344, -2.886751345948133984, -5.000000000000000000 ) ) ;
#12994 = B_SPLINE_CURVE_WITH_KNOTS ( 'NONE', 3,
 ( #15699, #2278, #7055, #11263, #13038 ),
 .UNSPECIFIED., .F., .F.,
 ( 4, 1, 4 ),
 ( 5.640274452250024914E-20, 0.002309401076758505356, 0.004618802153517010713 ),
 .UNSPECIFIED. ) ;
#12995 = ORIENTED_EDGE ( 'NONE', *, *, #17190, .T. ) ;
#12996 = EDGE_CURVE ( 'NONE', #14540, #5162, #7362, .T. ) ;
#12997 = CONICAL_SURFACE ( 'NONE', #8287, 4.000000000000000000, 0.8911886515913786111 ) ;
#12998 = EDGE_CURVE ( 'NONE', #4387, #16121, #16214, .T. ) ;
#12999 = ORIENTED_EDGE ( 'NONE', *, *, #1368, .T. ) ;
#13000 = CARTESIAN_POINT ( 'NONE',  ( -2.321707774797442170, -4.824281976789052351, -0.8000000000000000444 ) ) ;
#13001 =( LENGTH_UNIT ( ) NAMED_UNIT ( * ) SI_UNIT ( .MILLI., .METRE. ) );
#13002 = ORIENTED_EDGE ( 'NONE', *, *, #1317, .F. ) ;
#13003 = ADVANCED_FACE ( 'NONE', ( #10487 ), #7649, .T. ) ;
#13004 = CARTESIAN_POINT ( 'NONE',  ( 55.94051828345050836, 57.79948385550238754, -4.345558710429104465 ) ) ;
#13005 = CARTESIAN_POINT ( 'NONE',  ( -18.02113032590304442, -26.18033988749903074, -9.000000000000000000 ) ) ;
#13006 = ORIENTED_EDGE ( 'NONE', *, *, #4836, .T. ) ;
#13007 = VERTEX_POINT ( 'NONE', #4622 ) ;
#13008 = CARTESIAN_POINT ( 'NONE',  ( -5.560781378645573980, 0.000000000000000000, -4.000000000000000000 ) ) ;
#13009 = CIRCLE ( 'NONE', #15204, 2.649999999999985700 ) ;
#13010 = ORIENTED_EDGE ( 'NONE', *, *, #79, .F. ) ;
#13011 = DIRECTION ( 'NONE',  ( 1.000000000000000000, 0.000000000000000000, 0.000000000000000000 ) ) ;
#13012 = ORIENTED_EDGE ( 'NONE', *, *, #4788, .F. ) ;
#13013 = CARTESIAN_POINT ( 'NONE',  ( 47.70284917648453415, 49.39948385550238896, -6.992620115222774047 ) ) ;
#13014 = VECTOR ( 'NONE', #393, 1000.000000000000000 ) ;
#13015 = CARTESIAN_POINT ( 'NONE',  ( 0.000000000000000000, 0.000000000000000000, -25.03750572909317285 ) ) ;
#13016 = CARTESIAN_POINT ( 'NONE',  ( 55.96859303347802239, 48.80051614449766362, -4.306917132069484566 ) ) ;
#13017 = CARTESIAN_POINT ( 'NONE',  ( -154.8532481325730998, -18.99730707969839116, 15.00000000000000000 ) ) ;
#13018 = FACE_OUTER_BOUND ( 'NONE', #5101, .T. ) ;
#13019 = DIRECTION ( 'NONE',  ( 0.000000000000000000, 0.000000000000000000, 1.000000000000000000 ) ) ;
#13020 = AXIS2_PLACEMENT_3D ( 'NONE', #2045, #6640, #17050 ) ;
#13021 = EDGE_LOOP ( 'NONE', ( #3970, #16536, #9188, #2678 ) ) ;
#13022 = ORIENTED_EDGE ( 'NONE', *, *, #5099, .T. ) ;
#13023 = DIRECTION ( 'NONE',  ( -1.000000000000000000, 0.000000000000000000, 0.000000000000000000 ) ) ;
#13024 =( NAMED_UNIT ( * ) PLANE_ANGLE_UNIT ( ) SI_UNIT ( $, .RADIAN. ) );
#13025 = CARTESIAN_POINT ( 'NONE',  ( -154.9999999999999716, -14.99999999999999645, -15.79999999999999893 ) ) ;
#13026 = AXIS2_PLACEMENT_3D ( 'NONE', #865, #14577, #11348 ) ;
#13027 = LINE ( 'NONE', #19034, #2469 ) ;
#13028 = ORIENTED_EDGE ( 'NONE', *, *, #10485, .F. ) ;
#13029 = CARTESIAN_POINT ( 'NONE',  ( 6.362374563307939823, 3.415000007733389076, 4.302769906042884784 ) ) ;
#13030 = EDGE_CURVE ( 'NONE', #16278, #606, #2456, .T. ) ;
#13031 = ORIENTED_EDGE ( 'NONE', *, *, #16374, .F. ) ;
#13032 = ORIENTED_EDGE ( 'NONE', *, *, #710, .T. ) ;
#13033 = ADVANCED_FACE ( 'NONE', ( #1585 ), #10582, .T. ) ;
#13034 = LINE ( 'NONE', #987, #15986 ) ;
#13035 = DIRECTION ( 'NONE',  ( 1.000000000000000000, 0.000000000000000000, 0.000000000000000000 ) ) ;
#13036 = APPLICATION_CONTEXT ( 'automotive_design' ) ;
#13037 = CARTESIAN_POINT ( 'NONE',  ( 55.69932041026405045, 49.10051614449766788, 1.875703265242156359 ) ) ;
#13038 = CARTESIAN_POINT ( 'NONE',  ( 4.000000000000000000, -2.309401076758514915, -3.433295621305383349 ) ) ;
#13039 = CARTESIAN_POINT ( 'NONE',  ( 2.000000000000000000, 1.773042676681340524, -2.059984127722458425E-15 ) ) ;
#13040 = CARTESIAN_POINT ( 'NONE',  ( 53.50833635130540955, 53.69948385550240744, -4.867452303228209765 ) ) ;
#13041 = DIRECTION ( 'NONE',  ( -0.000000000000000000, 0.000000000000000000, -1.000000000000000000 ) ) ;
#13042 = CARTESIAN_POINT ( 'NONE',  ( 55.94051828345050836, 47.79948385550240886, -4.345558710429104465 ) ) ;
#13043 = CARTESIAN_POINT ( 'NONE',  ( 50.02271294988505446, 44.50051614449765935, -8.000000000000001776 ) ) ;
#13044 = CYLINDRICAL_SURFACE ( 'NONE', #16283, 5.999999999999977796 ) ;
#13045 = B_SPLINE_CURVE_WITH_KNOTS ( 'NONE', 3,
 ( #10021, #13627, #14805, #5892, #18159 ),
 .UNSPECIFIED., .F., .F.,
 ( 4, 1, 4 ),
 ( 0.000000000000000000, 0.002020725942163692675, 0.004041451884327385349 ),
 .UNSPECIFIED. ) ;
#13046 = DIRECTION ( 'NONE',  ( 0.000000000000000000, 0.000000000000000000, 1.000000000000000000 ) ) ;
#13047 = AXIS2_PLACEMENT_3D ( 'NONE', #12287, #4655, #233 ) ;
#13048 = DIRECTION ( 'NONE',  ( 0.000000000000000000, 0.000000000000000000, 1.000000000000000000 ) ) ;
#13049 = ORIENTED_EDGE ( 'NONE', *, *, #8553, .F. ) ;
#13050 = EDGE_CURVE ( 'NONE', #1122, #4165, #17764, .T. ) ;
#13051 = AXIS2_PLACEMENT_3D ( 'NONE', #13638, #17978, #19266 ) ;
#13052 = PRODUCT ( 'idle roller', 'idle roller', '', ( #13726 ) ) ;
#13053 = DIRECTION ( 'NONE',  ( 0.000000000000000000, 0.000000000000000000, -1.000000000000000000 ) ) ;
#13054 = CARTESIAN_POINT ( 'NONE',  ( 45.90387839640208512, 50.30051614449766362, -5.676469297603124353 ) ) ;
#13055 = CIRCLE ( 'NONE', #16189, 1.000000000000000000 ) ;
#13056 = CARTESIAN_POINT ( 'NONE',  ( -154.9999999999999716, -14.99999999999999645, 15.00000000000000000 ) ) ;
#13057 = DIRECTION ( 'NONE',  ( 1.000000000000000000, 0.000000000000000000, 0.000000000000000000 ) ) ;
#13058 = ORIENTED_EDGE ( 'NONE', *, *, #17206, .T. ) ;
#13059 = CIRCLE ( 'NONE', #8679, 15.00000000000000000 ) ;
#13060 = CARTESIAN_POINT ( 'NONE',  ( 2.000000000000000000, -1.773042676681341856, 2.276824562219559311E-15 ) ) ;
#13061 = LINE ( 'NONE', #11291, #15264 ) ;
#13062 = CARTESIAN_POINT ( 'NONE',  ( 44.05948171654949874, 52.79948385550240175, 4.345558710429105354 ) ) ;
#13063 = CARTESIAN_POINT ( 'NONE',  ( -154.9999999999999716, -14.99999999999999645, -15.00000000000000000 ) ) ;
#13064 = CARTESIAN_POINT ( 'NONE',  ( 54.68390685589039890, 63.30051614449767072, 6.485486291978072693 ) ) ;
#13065 = CARTESIAN_POINT ( 'NONE',  ( -4.211140560182196957, 2.431303136016537803, -3.745885042887433514 ) ) ;
#13066 = CARTESIAN_POINT ( 'NONE',  ( 50.02271294988505446, 48.50051614449765935, -7.000000000000000888 ) ) ;
#13067 = AXIS2_PLACEMENT_3D ( 'NONE', #5489, #19046, #11264 ) ;
#13068 = DIRECTION ( 'NONE',  ( 0.000000000000000000, 0.000000000000000000, -1.000000000000000000 ) ) ;
#13069 = ORIENTED_EDGE ( 'NONE', *, *, #8499, .T. ) ;
#13070 = VECTOR ( 'NONE', #873, 1000.000000000000000 ) ;
#13071 = ORIENTED_EDGE ( 'NONE', *, *, #3762, .T. ) ;
#13072 = CARTESIAN_POINT ( 'NONE',  ( 2.449293598294706513E-15, -20.00000000000000000, 9.000000000000000000 ) ) ;
#13073 = VECTOR ( 'NONE', #11323, 1000.000000000000000 ) ;
#13074 = VERTEX_POINT ( 'NONE', #17969 ) ;
#13075 = DIRECTION ( 'NONE',  ( -1.000000000000000000, 0.000000000000000000, -0.000000000000000000 ) ) ;
#13076 = VERTEX_POINT ( 'NONE', #3158 ) ;
#13077 = CARTESIAN_POINT ( 'NONE',  ( -14.86289650954790886, -6.617387872822862782, 9.000000000000000000 ) ) ;
#13078 = ORIENTED_EDGE ( 'NONE', *, *, #15806, .F. ) ;
#13079 = DIRECTION ( 'NONE',  ( -1.000000000000000000, 0.000000000000000000, 0.000000000000000000 ) ) ;
#13080 = VERTEX_POINT ( 'NONE', #2870 ) ;
#13081 = AXIS2_PLACEMENT_3D ( 'NONE', #18002, #4562, #1626 ) ;
#13082 = CARTESIAN_POINT ( 'NONE',  ( 43.18075615816989199, 59.19948385550240744, -4.924951120819313743 ) ) ;
#13083 = DIRECTION ( 'NONE',  ( 0.000000000000000000, 0.000000000000000000, 1.000000000000000000 ) ) ;
#13084 = CIRCLE ( 'NONE', #14962, 0.7500000000000000000 ) ;
#13085 = CARTESIAN_POINT ( 'NONE',  ( 51.97223112728254790, 50.39948385550241738, 5.992620115222778487 ) ) ;
#13086 = LINE ( 'NONE', #7304, #15110 ) ;
#13087 = CARTESIAN_POINT ( 'NONE',  ( 1.925929944387235853E-31, 15.00000000000001599, 15.00000000000000000 ) ) ;
#13088 = CARTESIAN_POINT ( 'NONE',  ( 41.58830220609386430, 48.00051614449766646, -0.02388180880514929535 ) ) ;
#13089 = CARTESIAN_POINT ( 'NONE',  ( 55.08986747509849380, 51.20051614449766220, 3.727524721679155384 ) ) ;
#13090 = CARTESIAN_POINT ( 'NONE',  ( -0.9999999999999976685, -20.00000000000000000, 8.999999999999998224 ) ) ;
#13091 = DIRECTION ( 'NONE',  ( 0.000000000000000000, 0.8660254037844375974, -0.5000000000000018874 ) ) ;
#13092 = ORIENTED_EDGE ( 'NONE', *, *, #15145, .T. ) ;
#13093 = VERTEX_POINT ( 'NONE', #112 ) ;
#13094 = FACE_OUTER_BOUND ( 'NONE', #3211, .T. ) ;
#13095 =( LENGTH_UNIT ( ) NAMED_UNIT ( * ) SI_UNIT ( .MILLI., .METRE. ) );
#13096 = ORIENTED_EDGE ( 'NONE', *, *, #17927, .F. ) ;
#13097 = VECTOR ( 'NONE', #9492, 1000.000000000000000 ) ;
#13098 = EDGE_CURVE ( 'NONE', #10464, #11251, #18118, .T. ) ;
#13099 = VECTOR ( 'NONE', #2459, 1000.000000000000000 ) ;
#13100 = CARTESIAN_POINT ( 'NONE',  ( 56.65037692655918988, 55.89948385550240317, -2.184720259617163762 ) ) ;
#13101 = VERTEX_POINT ( 'NONE', #10395 ) ;
#13102 = VERTEX_POINT ( 'NONE', #9016 ) ;
#13103 = LINE ( 'NONE', #16060, #13337 ) ;
#13104 = FACE_OUTER_BOUND ( 'NONE', #15291, .T. ) ;
#13105 = ADVANCED_FACE ( 'NONE', ( #1481 ), #10250, .T. ) ;
#13106 = ORIENTED_EDGE ( 'NONE', *, *, #4258, .F. ) ;
#13107 = LINE ( 'NONE', #18824, #2575 ) ;
#13108 = ORIENTED_EDGE ( 'NONE', *, *, #10456, .F. ) ;
#13109 = CARTESIAN_POINT ( 'NONE',  ( -1.257172072275743346, 3.892973519171203378, -3.433252694550776862 ) ) ;
#13110 = EDGE_CURVE ( 'NONE', #11651, #15728, #4324, .T. ) ;
#13111 = EDGE_CURVE ( 'NONE', #8262, #16221, #17482, .T. ) ;
#13112 = CARTESIAN_POINT ( 'NONE',  ( 42.63976443033212860, 50.99948385550240459, 0.02388180880522514787 ) ) ;
#13113 = DIRECTION ( 'NONE',  ( 0.6040472319084893016, -0.7969485188038759604, -1.107688701425240251E-17 ) ) ;
#13114 = CARTESIAN_POINT ( 'NONE',  ( 56.65037692655921120, 51.10051614449766078, 2.184720259617097593 ) ) ;
#13115 = CARTESIAN_POINT ( 'NONE',  ( 16.79901371501595975, -30.85325472854598416, -9.000000000000000000 ) ) ;
#13116 = AXIS2_PLACEMENT_3D ( 'NONE', #7911, #6637, #562 ) ;
#13117 = AXIS2_PLACEMENT_3D ( 'NONE', #12321, #15266, #274 ) ;
#13118 = ADVANCED_FACE ( 'NONE', ( #9122 ), #1385, .F. ) ;
#13119 = DIRECTION ( 'NONE',  ( 1.000000000000000000, 0.000000000000000000, -0.000000000000000000 ) ) ;
#13120 = ORIENTED_EDGE ( 'NONE', *, *, #17798, .T. ) ;
#13121 = ORIENTED_EDGE ( 'NONE', *, *, #3904, .F. ) ;
#13122 = CARTESIAN_POINT ( 'NONE',  ( 2.449293598294706513E-15, -20.00000000000000000, 15.00000000000000355 ) ) ;
#13123 = ADVANCED_FACE ( 'NONE', ( #12156 ), #270, .T. ) ;
#13124 = DIRECTION ( 'NONE',  ( -1.387778780781445676E-16, 1.000000000000000000, 0.000000000000000000 ) ) ;
#13125 = EDGE_CURVE ( 'NONE', #12007, #7897, #12777, .T. ) ;
#13126 = CARTESIAN_POINT ( 'NONE',  ( 19.30627432446641123, -14.77814480204120784, 0.000000000000000000 ) ) ;
#13127 = EDGE_LOOP ( 'NONE', ( #568, #13467, #14179, #13969 ) ) ;
#13128 = CARTESIAN_POINT ( 'NONE',  ( 6.327632967268630004, 3.313549392874629795, 4.260764098153893897 ) ) ;
#13129 = AXIS2_PLACEMENT_3D ( 'NONE', #3673, #9637, #15635 ) ;
#13130 = CIRCLE ( 'NONE', #6542, 7.500000000000000888 ) ;
#13131 = VERTEX_POINT ( 'NONE', #13240 ) ;
#13132 = ORIENTED_EDGE ( 'NONE', *, *, #2839, .F. ) ;
#13133 = DIRECTION ( 'NONE',  ( 1.000000000000000000, 0.000000000000000000, 0.000000000000000000 ) ) ;
#13134 = CIRCLE ( 'NONE', #7185, 0.7500000000000000000 ) ;
#13135 = DIRECTION ( 'NONE',  ( -0.000000000000000000, 1.000000000000000000, -0.000000000000000000 ) ) ;
#13136 = CARTESIAN_POINT ( 'NONE',  ( 53.50833635130544508, 49.30051614449766362, 4.867452303228181343 ) ) ;
#13137 = CYLINDRICAL_SURFACE ( 'NONE', #11083, 4.000000000000000000 ) ;
#13138 = DIRECTION ( 'NONE',  ( 1.000000000000000000, 0.000000000000000000, 0.000000000000000000 ) ) ;
#13139 = CARTESIAN_POINT ( 'NONE',  ( 53.54508667620428497, 52.29948385550240886, 4.840751629271157874 ) ) ;
#13140 = CYLINDRICAL_SURFACE ( 'NONE', #5641, 2.396904916527700102 ) ;
#13141 = CARTESIAN_POINT ( 'NONE',  ( 43.33558569842703179, 49.09948385550240602, -2.141517661632099223 ) ) ;
#13142 = VECTOR ( 'NONE', #15712, 1000.000000000000000 ) ;
#13143 = CARTESIAN_POINT ( 'NONE',  ( 45.31609314410960820, 48.30051614449765651, -6.485486291978072693 ) ) ;
#13144 = DIRECTION ( 'NONE',  ( 1.000000000000000000, 0.000000000000000000, 0.000000000000000000 ) ) ;
#13145 = CARTESIAN_POINT ( 'NONE',  ( 4.000000000000000000, 0.000000000000000000, 0.000000000000000000 ) ) ;
#13146 = APPLICATION_PROTOCOL_DEFINITION ( 'draft international standard', 'automotive_design', 1998, #18817 ) ;
#13147 = TOROIDAL_SURFACE ( 'NONE', #12837, 4.100000000000000533, 0.1000000000000001582 ) ;
#13148 = EDGE_LOOP ( 'NONE', ( #19416, #6238 ) ) ;
#13149 = CARTESIAN_POINT ( 'NONE',  ( -0.5636800770129166693, -4.293361309317430319, -3.531542292955206275 ) ) ;
#13150 = CARTESIAN_POINT ( 'NONE',  ( 0.1999999999999987899, 0.000000000000000000, 0.000000000000000000 ) ) ;
#13151 = AXIS2_PLACEMENT_3D ( 'NONE', #12065, #6285, #18068 ) ;
#13152 = CARTESIAN_POINT ( 'NONE',  ( -0.3461262719736137305, 4.658553426539289610, -3.671615880910373608 ) ) ;
#13153 = CARTESIAN_POINT ( 'NONE',  ( -62.49999999999997158, 45.00000000000001421, -15.00000000000000000 ) ) ;
#13154 = AXIS2_PLACEMENT_3D ( 'NONE', #17759, #7353, #8017 ) ;
#13155 = ORIENTED_EDGE ( 'NONE', *, *, #892, .F. ) ;
#13156 = VECTOR ( 'NONE', #72, 1000.000000000000000 ) ;
#13157 = DIRECTION ( 'NONE',  ( -1.000000000000000000, 0.000000000000000000, -0.000000000000000000 ) ) ;
#13158 = CARTESIAN_POINT ( 'NONE',  ( 2.836893136758676270, 3.208949435745843903, -3.505054077164911241 ) ) ;
#13159 = CARTESIAN_POINT ( 'NONE',  ( 44.03140696652192787, 53.19948385550238612, -4.306917132069425058 ) ) ;
#13160 = AXIS2_PLACEMENT_3D ( 'NONE', #18209, #11102, #14040 ) ;
#13161 = LINE ( 'NONE', #12873, #15462 ) ;
#13162 = CARTESIAN_POINT ( 'NONE',  ( 43.20883090819745576, 48.79948385550240175, 4.963592699179006473 ) ) ;
#13163 = DIRECTION ( 'NONE',  ( 0.000000000000000000, 0.000000000000000000, 1.000000000000000000 ) ) ;
#13164 = CARTESIAN_POINT ( 'NONE',  ( 43.33558569842706021, 47.90051614449765793, 2.141517661632167169 ) ) ;
#13165 = EDGE_CURVE ( 'NONE', #17750, #3558, #7779, .T. ) ;
#13166 = DIRECTION ( 'NONE',  ( -1.000000000000000000, -0.000000000000000000, -0.000000000000000000 ) ) ;
#13167 = EDGE_LOOP ( 'NONE', ( #11545, #2757, #3584 ) ) ;
#13168 = EDGE_CURVE ( 'NONE', #3999, #3553, #14808, .T. ) ;
#13169 = CIRCLE ( 'NONE', #10965, 3.500000000000000000 ) ;
#13170 = AXIS2_PLACEMENT_3D ( 'NONE', #13367, #7484, #7194 ) ;
#13171 = EDGE_LOOP ( 'NONE', ( #4552, #12821, #12739, #8071 ) ) ;
#13172 = DIRECTION ( 'NONE',  ( 1.000000000000000000, 0.000000000000000000, 0.000000000000000000 ) ) ;
#13173 = VERTEX_POINT ( 'NONE', #14908 ) ;
#13174 = CARTESIAN_POINT ( 'NONE',  ( 4.688877333453707941, -18.97314589549297281, 9.000000000000000000 ) ) ;
#13175 = AXIS2_PLACEMENT_3D ( 'NONE', #1406, #9140, #2080 ) ;
#13176 = ORIENTED_EDGE ( 'NONE', *, *, #16359, .F. ) ;
#13177 = CARTESIAN_POINT ( 'NONE',  ( -154.9999999999999716, -14.99999999999999645, 15.00000000000000000 ) ) ;
#13178 = VERTEX_POINT ( 'NONE', #6003 ) ;
#13179 = CARTESIAN_POINT ( 'NONE',  ( 0.04201760816084261496, -0.9730571234389092661, -5.000000000000000888 ) ) ;
#13180 = EDGE_LOOP ( 'NONE', ( #16356, #15179, #5119, #8885, #13022, #8345, #18505 ) ) ;
#13181 = CARTESIAN_POINT ( 'NONE',  ( 57.61547081786812896, 60.09948385550240602, 2.450534656007040901 ) ) ;
#13182 = AXIS2_PLACEMENT_3D ( 'NONE', #10855, #14278, #6446 ) ;
#13183 = CARTESIAN_POINT ( 'NONE',  ( 50.00000000000000000, 15.00000000000000000, 0.000000000000000000 ) ) ;
#13184 = CARTESIAN_POINT ( 'NONE',  ( 44.91013252490152752, 52.79948385550240175, 3.727524721679198461 ) ) ;
#13185 = CARTESIAN_POINT ( 'NONE',  ( 6.196878017913831194, -5.292377467571572680, 0.8333333333333327042 ) ) ;
#13186 = LINE ( 'NONE', #17623, #872 ) ;
#13187 = AXIS2_PLACEMENT_3D ( 'NONE', #963, #3906, #6936 ) ;
#13188 = CIRCLE ( 'NONE', #4426, 20.00000000000000000 ) ;
#13189 = CARTESIAN_POINT ( 'NONE',  ( 45.27934281921082516, 49.70051614449766220, 6.458785618021089192 ) ) ;
#13190 = CARTESIAN_POINT ( 'NONE',  ( 53.50833635130544508, 51.30051614449765651, 4.867452303228181343 ) ) ;
#13191 = CARTESIAN_POINT ( 'NONE',  ( 4.175813232069148562, -2.061359961916374051, -3.570380186727397653 ) ) ;
#13192 = DIRECTION ( 'NONE',  ( 1.000000000000000000, 0.000000000000000000, 0.000000000000000000 ) ) ;
#13193 = ORIENTED_EDGE ( 'NONE', *, *, #7955, .F. ) ;
#13194 = ORIENTED_EDGE ( 'NONE', *, *, #14664, .F. ) ;
#13195 = LINE ( 'NONE', #12006, #12823 ) ;
#13196 = EDGE_LOOP ( 'NONE', ( #4593, #15657, #10317, #14085 ) ) ;
#13197 = CARTESIAN_POINT ( 'NONE',  ( 47.70284917648453415, 63.39948385550240317, -6.992620115222774047 ) ) ;
#13198 = DIRECTION ( 'NONE',  ( 0.000000000000000000, 0.000000000000000000, 1.000000000000000000 ) ) ;
#13199 = ORIENTED_EDGE ( 'NONE', *, *, #1562, .F. ) ;
#13200 = ORIENTED_EDGE ( 'NONE', *, *, #7704, .T. ) ;
#13201 = DIRECTION ( 'NONE',  ( -0.8191520442889875797, 1.003171929053519570E-16, 0.5735764363510522656 ) ) ;
#13202 = CARTESIAN_POINT ( 'NONE',  ( 52.25172492374522903, 45.59948385550240602, -7.007379884777227730 ) ) ;
#13203 = VECTOR ( 'NONE', #7904, 1000.000000000000000 ) ;
#13204 = EDGE_LOOP ( 'NONE', ( #15858, #19105, #5370, #7847 ) ) ;
#13205 = CARTESIAN_POINT ( 'NONE',  ( 73.00000000000000000, 3.000000000000000000, 5.999999999999998224 ) ) ;
#13206 = ORIENTED_EDGE ( 'NONE', *, *, #6384, .T. ) ;
#13207 = FACE_OUTER_BOUND ( 'NONE', #14450, .T. ) ;
#13208 = CARTESIAN_POINT ( 'NONE',  ( 54.13287192849676188, 54.29948385550240886, 5.649768623646098220 ) ) ;
#13209 = DIRECTION ( 'NONE',  ( -1.000000000000000000, 0.000000000000000000, 0.000000000000000000 ) ) ;
#13210 = CARTESIAN_POINT ( 'NONE',  ( 52.29715082351538769, 48.60051614449766788, -6.992620115222796251 ) ) ;
#13211 = CARTESIAN_POINT ( 'NONE',  ( -0.1085714285714285687, -3.798448662927795372, 0.000000000000000000 ) ) ;
#13212 = ADVANCED_FACE ( 'NONE', ( #11965 ), #8021, .F. ) ;
#13213 = DIRECTION ( 'NONE',  ( -0.000000000000000000, -0.000000000000000000, 1.000000000000000000 ) ) ;
#13214 = DIRECTION ( 'NONE',  ( 1.000000000000000000, 0.000000000000000000, 0.000000000000000000 ) ) ;
#13215 = PRODUCT_DEFINITION ( 'UNKNOWN', '', #15757, #2050 ) ;
#13216 = ORIENTED_EDGE ( 'NONE', *, *, #6633, .T. ) ;
#13217 = ORIENTED_EDGE ( 'NONE', *, *, #12671, .T. ) ;
#13218 = DIRECTION ( 'NONE',  ( 0.000000000000000000, 1.000000000000000000, 0.000000000000000000 ) ) ;
#13219 = DIRECTION ( 'NONE',  ( 0.000000000000000000, 0.000000000000000000, 1.000000000000000000 ) ) ;
#13220 = CARTESIAN_POINT ( 'NONE',  ( -54.99999999999996447, -6.999999999999985789, -10.00000000000000000 ) ) ;
#13221 = VERTEX_POINT ( 'NONE', #12541 ) ;
#13222 = DIRECTION ( 'NONE',  ( -1.000000000000000000, 0.000000000000000000, 0.000000000000000000 ) ) ;
#13223 = EDGE_CURVE ( 'NONE', #1251, #4202, #7154, .T. ) ;
#13224 = ADVANCED_FACE ( 'NONE', ( #6457, #16685 ), #18446, .T. ) ;
#13225 = VECTOR ( 'NONE', #17013, 1000.000000000000000 ) ;
#13226 = ORIENTED_EDGE ( 'NONE', *, *, #5683, .T. ) ;
#13227 = ORIENTED_EDGE ( 'NONE', *, *, #12148, .F. ) ;
#13228 = DIRECTION ( 'NONE',  ( 0.000000000000000000, 0.000000000000000000, 1.000000000000000000 ) ) ;
#13229 = DIRECTION ( 'NONE',  ( 0.000000000000000000, 0.000000000000000000, -1.000000000000000000 ) ) ;
#13230 = CARTESIAN_POINT ( 'NONE',  ( 55.11794222512599362, 46.80051614449766362, -3.688883143319583446 ) ) ;
#13231 = DIRECTION ( 'NONE',  ( 0.000000000000000000, 0.000000000000000000, 1.000000000000000000 ) ) ;
#13232 = EDGE_CURVE ( 'NONE', #5072, #8263, #14335, .T. ) ;
#13233 = DIRECTION ( 'NONE',  ( 1.000000000000000000, 0.000000000000000000, 0.000000000000000000 ) ) ;
#13234 = EDGE_CURVE ( 'NONE', #6250, #7579, #4329, .T. ) ;
#13235 = CARTESIAN_POINT ( 'NONE',  ( 50.02271294988511841, 52.49948385550241170, 6.000000000000000888 ) ) ;
#13236 = DIRECTION ( 'NONE',  ( -4.082155997157844188E-16, 1.000000000000000000, 0.000000000000000000 ) ) ;
#13237 = CARTESIAN_POINT ( 'NONE',  ( 49.97728705011488159, 49.49948385550240459, -7.000000000000000888 ) ) ;
#13238 = CARTESIAN_POINT ( 'NONE',  ( 57.60143344285435774, 49.10051614449766788, 2.493737253992045044 ) ) ;
#13239 = CARTESIAN_POINT ( 'NONE',  ( 4.175326769692856210, -2.060699556488920337, -3.569236330973475813 ) ) ;
#13240 = CARTESIAN_POINT ( 'NONE',  ( -74.99999999999997158, -3.000000000000000000, -5.999999999999998224 ) ) ;
#13241 = EDGE_CURVE ( 'NONE', #5231, #16758, #1520, .T. ) ;
#13242 = CARTESIAN_POINT ( 'NONE',  ( -154.9999999999999716, -14.99999999999999645, -7.750000000000001776 ) ) ;
#13243 = EDGE_CURVE ( 'NONE', #3598, #13512, #9584, .T. ) ;
#13244 = AXIS2_PLACEMENT_3D ( 'NONE', #19256, #14810, #19162 ) ;
#13245 = ORIENTED_EDGE ( 'NONE', *, *, #4436, .F. ) ;
#13246 = DIRECTION ( 'NONE',  ( 9.858538378746663627E-23, -5.031452844637890958E-23, 1.000000000000000000 ) ) ;
#13247 = EDGE_CURVE ( 'NONE', #13385, #19390, #14975, .T. ) ;
#13248 = LINE ( 'NONE', #16103, #5958 ) ;
#13249 = FACE_OUTER_BOUND ( 'NONE', #12480, .T. ) ;
#13250 = DIRECTION ( 'NONE',  ( -0.000000000000000000, -0.000000000000000000, -1.000000000000000000 ) ) ;
#13251 = CARTESIAN_POINT ( 'NONE',  ( 6.527192678185834041, 2.941622124011172623, 5.095038975455953079 ) ) ;
#13252 = LINE ( 'NONE', #16309, #1395 ) ;
#13253 = DIRECTION ( 'NONE',  ( 0.000000000000000000, 0.000000000000000000, -1.000000000000000000 ) ) ;
#13254 = CARTESIAN_POINT ( 'NONE',  ( 54.13287192849676188, 52.29948385550240886, 5.649768623646098220 ) ) ;
#13255 = CARTESIAN_POINT ( 'NONE',  ( -154.9999999999999716, -14.99999999999999645, -3.999999999999999112 ) ) ;
#13256 = CARTESIAN_POINT ( 'NONE',  ( 41.58830220609386430, 52.99948385550241170, 0.02388180880523263147 ) ) ;
#13257 = APPLICATION_CONTEXT ( 'automotive_design' ) ;
#13258 = DIRECTION ( 'NONE',  ( 0.000000000000000000, 0.000000000000000000, 1.000000000000000000 ) ) ;
#13259 = CARTESIAN_POINT ( 'NONE',  ( 44.05948171654945611, 48.20051614449764799, -4.345558710429044069 ) ) ;
#13260 = DIRECTION ( 'NONE',  ( -1.000000000000000000, -0.000000000000000000, -0.000000000000000000 ) ) ;
#13261 = ORIENTED_EDGE ( 'NONE', *, *, #13563, .T. ) ;
#13262 = CIRCLE ( 'NONE', #4200, 8.099999999999999645 ) ;
#13263 = ORIENTED_EDGE ( 'NONE', *, *, #17698, .F. ) ;
#13264 = CARTESIAN_POINT ( 'NONE',  ( -62.49999999999997158, 45.00000000000001421, 9.999999999999998224 ) ) ;
#13265 = VERTEX_POINT ( 'NONE', #6275 ) ;
#13266 = AXIS2_PLACEMENT_3D ( 'NONE', #9135, #4447, #15213 ) ;
#13267 = CARTESIAN_POINT ( 'NONE',  ( -29.99999999999999645, 40.00000000000000000, 0.000000000000000000 ) ) ;
#13268 = ORIENTED_EDGE ( 'NONE', *, *, #13395, .T. ) ;
#13269 = DIRECTION ( 'NONE',  ( -0.5000000000000041078, 0.8660254037844362651, 0.000000000000000000 ) ) ;
#13270 = EDGE_CURVE ( 'NONE', #2819, #12421, #19278, .T. ) ;
#13271 = ORIENTED_EDGE ( 'NONE', *, *, #12189, .F. ) ;
#13272 = DIRECTION ( 'NONE',  ( 0.000000000000000000, 0.000000000000000000, -1.000000000000000000 ) ) ;
#13273 = ORIENTED_EDGE ( 'NONE', *, *, #13755, .F. ) ;
#13274 = CARTESIAN_POINT ( 'NONE',  ( 56.79116909180255135, 59.79948385550240175, -4.963592699179005585 ) ) ;
#13275 = PLANE ( 'NONE',  #15778 ) ;
#13276 = EDGE_CURVE ( 'NONE', #3696, #15553, #15602, .T. ) ;
#13277 = CARTESIAN_POINT ( 'NONE',  ( 48.07319477248768180, 54.59948385550240602, 6.007379884777225953 ) ) ;
#13278 = VECTOR ( 'NONE', #12670, 1000.000000000000000 ) ;
#13279 = DIRECTION ( 'NONE',  ( 0.000000000000000000, 0.000000000000000000, -1.000000000000000000 ) ) ;
#13280 = CARTESIAN_POINT ( 'NONE',  ( 45.15499999999999403, 0.000000000000000000, 0.000000000000000000 ) ) ;
#13281 = CARTESIAN_POINT ( 'NONE',  ( 45.31609314410960820, 52.30051614449766362, -6.485486291978072693 ) ) ;
#13282 = VECTOR ( 'NONE', #6569, 1000.000000000000000 ) ;
#13283 = CARTESIAN_POINT ( 'NONE',  ( 48.07319477248762496, 52.40051614449767214, -6.007379884777208190 ) ) ;
#13284 = DIRECTION ( 'NONE',  ( 0.000000000000000000, 0.000000000000000000, -1.000000000000000000 ) ) ;
#13285 = DIRECTION ( 'NONE',  ( -0.000000000000000000, 0.000000000000000000, -1.000000000000000000 ) ) ;
#13286 = ORIENTED_EDGE ( 'NONE', *, *, #7598, .T. ) ;
#13287 = ORIENTED_EDGE ( 'NONE', *, *, #4492, .F. ) ;
#13288 = LINE ( 'NONE', #19405, #17525 ) ;
#13289 = ORIENTED_EDGE ( 'NONE', *, *, #8064, .F. ) ;
#13290 = DIRECTION ( 'NONE',  ( 2.191393683118470056E-17, 7.538405132783724027E-17, 1.000000000000000000 ) ) ;
#13291 = FACE_OUTER_BOUND ( 'NONE', #4880, .T. ) ;
#13292 = ORIENTED_EDGE ( 'NONE', *, *, #361, .T. ) ;
#13293 = CIRCLE ( 'NONE', #12351, 2.649999999999985700 ) ;
#13294 = FACE_OUTER_BOUND ( 'NONE', #6801, .T. ) ;
#13295 = CARTESIAN_POINT ( 'NONE',  ( 56.66441430157296821, 48.09948385550240602, 2.141517661632100111 ) ) ;
#13296 = VERTEX_POINT ( 'NONE', #18354 ) ;
#13297 = CARTESIAN_POINT ( 'NONE',  ( -62.49999999999997158, 32.50000000000001421, 15.00000000000000178 ) ) ;
#13298 = ORIENTED_EDGE ( 'NONE', *, *, #783, .F. ) ;
#13299 = CARTESIAN_POINT ( 'NONE',  ( -154.9999999999999716, -14.99999999999999645, 3.999999999999999112 ) ) ;
#13300 = VECTOR ( 'NONE', #15150, 1000.000000000000000 ) ;
#13301 = CARTESIAN_POINT ( 'NONE',  ( 56.65037692655918988, 57.89948385550240317, -2.184720259617163762 ) ) ;
#13302 = DIRECTION ( 'NONE',  ( 0.01780247661957949645, 0.9998415233556812165, -7.576222706442768103E-17 ) ) ;
#13303 = CARTESIAN_POINT ( 'NONE',  ( 45.90387839640208512, 50.30051614449766362, -5.676469297603124353 ) ) ;
#13304 = DIRECTION ( 'NONE',  ( 0.000000000000000000, 0.000000000000000000, 1.000000000000000000 ) ) ;
#13305 = FACE_OUTER_BOUND ( 'NONE', #17533, .T. ) ;
#13306 = CIRCLE ( 'NONE', #12674, 0.1000000000000002554 ) ;
#13307 = CARTESIAN_POINT ( 'NONE',  ( -4.000000000000000000, 2.471528634177585282, -3.686887442155186712 ) ) ;
#13308 = ORIENTED_EDGE ( 'NONE', *, *, #16599, .F. ) ;
#13309 = CIRCLE ( 'NONE', #1422, 3.500000000000000000 ) ;
#13310 = ORIENTED_EDGE ( 'NONE', *, *, #7806, .T. ) ;
#13311 = ORIENTED_EDGE ( 'NONE', *, *, #575, .T. ) ;
#13312 = DIRECTION ( 'NONE',  ( -0.000000000000000000, 0.000000000000000000, 1.000000000000000000 ) ) ;
#13313 = VECTOR ( 'NONE', #17873, 1000.000000000000000 ) ;
#13314 = CARTESIAN_POINT ( 'NONE',  ( 57.36023556966787851, 45.99948385550238328, -0.02388180880522424582 ) ) ;
#13315 = PRESENTATION_STYLE_ASSIGNMENT (( #18038 ) ) ;
#13316 = VERTEX_POINT ( 'NONE', #13997 ) ;
#13317 = DIRECTION ( 'NONE',  ( -0.000000000000000000, -0.000000000000000000, -1.000000000000000000 ) ) ;
#13318 = EDGE_LOOP ( 'NONE', ( #4208, #10433, #2185, #3852 ) ) ;
#13319 = EDGE_LOOP ( 'NONE', ( #15515, #256, #3106, #18121, #14860, #6368 ) ) ;
#13320 = CYLINDRICAL_SURFACE ( 'NONE', #13794, 1.000000000000000888 ) ;
#13321 = CARTESIAN_POINT ( 'NONE',  ( -54.99999999999996447, -14.99999999999998579, 10.00000000000000000 ) ) ;
#13322 = CARTESIAN_POINT ( 'NONE',  ( 51.97223112728249816, 48.60051614449766788, -5.992620115222793586 ) ) ;
#13323 = CARTESIAN_POINT ( 'NONE',  ( 0.08165819712377191120, -4.939961795957299451, -1.443735181952766400 ) ) ;
#13324 = CARTESIAN_POINT ( 'NONE',  ( 75.00000000000000000, 32.50000000000001421, 15.00000000000000000 ) ) ;
#13325 = CARTESIAN_POINT ( 'NONE',  ( 56.30877334542961421, 57.99948385550241170, -0.02388180880520959434 ) ) ;
#13326 = CARTESIAN_POINT ( 'NONE',  ( 4.141042297810615835, -2.227970268150433863, -3.687027686973623819 ) ) ;
#13327 = CARTESIAN_POINT ( 'NONE',  ( 57.36023556966787851, 53.99948385550239038, -0.02388180880522424582 ) ) ;
#13328 = CARTESIAN_POINT ( 'NONE',  ( 45.27934281921082516, 55.70051614449766220, 6.458785618021089192 ) ) ;
#13329 = CARTESIAN_POINT ( 'NONE',  ( 4.142654963991852846, -2.035398498734352746, -3.525413613457307971 ) ) ;
#13330 = DIRECTION ( 'NONE',  ( 1.000000000000000000, 0.000000000000000000, 0.000000000000000000 ) ) ;
#13331 = COLOUR_RGB ( '',0.8941176470588234615, 0.8941176470588234615, 0.8941176470588234615 ) ;
#13332 = EDGE_CURVE ( 'NONE', #16243, #6353, #10589, .T. ) ;
#13333 = CARTESIAN_POINT ( 'NONE',  ( -4.747884751462026820, -5.143694235355983579, -0.8000000000000000444 ) ) ;
#13334 = CARTESIAN_POINT ( 'NONE',  ( -54.99999999999996447, -14.99999999999998579, 20.60000000000000142 ) ) ;
#13335 = ORIENTED_EDGE ( 'NONE', *, *, #4008, .T. ) ;
#13336 = CARTESIAN_POINT ( 'NONE',  ( 0.6666666666666689611, 4.233901974057261874, -3.300726591567082480 ) ) ;
#13337 = VECTOR ( 'NONE', #18820, 1000.000000000000000 ) ;
#13338 = EDGE_CURVE ( 'NONE', #18235, #14101, #2160, .T. ) ;
#13339 = ADVANCED_FACE ( 'NONE', ( #686 ), #6657, .T. ) ;
#13340 = DIRECTION ( 'NONE',  ( 0.000000000000000000, 0.000000000000000000, 1.000000000000000000 ) ) ;
#13341 = EDGE_CURVE ( 'NONE', #14650, #12327, #15921, .T. ) ;
#13342 = DIRECTION ( 'NONE',  ( -0.000000000000000000, -0.000000000000000000, 1.000000000000000000 ) ) ;
#13343 = LINE ( 'NONE', #19365, #10557 ) ;
#13344 = FACE_OUTER_BOUND ( 'NONE', #9542, .T. ) ;
#13345 = LINE ( 'NONE', #6014, #6098 ) ;
#13346 = ADVANCED_FACE ( 'NONE', ( #13817 ), #7745, .T. ) ;
#13347 = ADVANCED_FACE ( 'NONE', ( #4812 ), #10776, .T. ) ;
#13348 = CARTESIAN_POINT ( 'NONE',  ( 3.973110223767137850, 2.263269463293572928E-11, 3.565797985667434222 ) ) ;
#13349 = CARTESIAN_POINT ( 'NONE',  ( 55.94051828345050836, 57.79948385550238754, -4.345558710429104465 ) ) ;
#13350 = CARTESIAN_POINT ( 'NONE',  ( 5.560781378645573980, 6.809993116116507654E-16, -4.000000000000000000 ) ) ;
#13351 = AXIS2_PLACEMENT_3D ( 'NONE', #15419, #8053, #4929 ) ;
#13352 = CARTESIAN_POINT ( 'NONE',  ( 41.58830220609386430, 54.99948385550239749, 0.02388180880523263147 ) ) ;
#13353 = DIRECTION ( 'NONE',  ( 1.000000000000000000, 0.000000000000000000, 0.000000000000000000 ) ) ;
#13354 = CARTESIAN_POINT ( 'NONE',  ( 57.36023556966787851, 51.00051614449763804, 0.02388180880515038476 ) ) ;
#13355 = DIRECTION ( 'NONE',  ( -0.000000000000000000, -0.000000000000000000, -1.000000000000000000 ) ) ;
#13356 = PRODUCT_DEFINITION_SHAPE ( 'NONE', 'NONE',  #9726 ) ;
#13357 = EDGE_LOOP ( 'NONE', ( #14741, #5554 ) ) ;
#13358 = ORIENTED_EDGE ( 'NONE', *, *, #19306, .T. ) ;
#13359 = CARTESIAN_POINT ( 'NONE',  ( 0.000000000000000000, 0.000000000000000000, 0.000000000000000000 ) ) ;
#13360 = ORIENTED_EDGE ( 'NONE', *, *, #12182, .T. ) ;
#13361 = EDGE_CURVE ( 'NONE', #5461, #14841, #9325, .T. ) ;
#13362 = AXIS2_PLACEMENT_3D ( 'NONE', #15417, #18477, #12465 ) ;
#13363 = EDGE_CURVE ( 'NONE', #10122, #88, #9877, .T. ) ;
#13364 = DIRECTION ( 'NONE',  ( 0.000000000000000000, -0.000000000000000000, 1.000000000000000000 ) ) ;
#13365 = VECTOR ( 'NONE', #3330, 1000.000000000000000 ) ;
#13366 = ORIENTED_EDGE ( 'NONE', *, *, #17739, .F. ) ;
#13367 = CARTESIAN_POINT ( 'NONE',  ( 13.99999999999999822, 0.000000000000000000, 0.000000000000000000 ) ) ;
#13368 = EDGE_LOOP ( 'NONE', ( #16417, #17513, #3877, #11239 ) ) ;
#13369 = CARTESIAN_POINT ( 'NONE',  ( -44.99999999999997158, -40.00000000000000000, -20.00000000000000000 ) ) ;
#13370 = ORIENTED_EDGE ( 'NONE', *, *, #9863, .F. ) ;
#13371 = CARTESIAN_POINT ( 'NONE',  ( 2.321707774797442170, -4.824281976789052351, -0.8000000000000000444 ) ) ;
#13372 = DIRECTION ( 'NONE',  ( 1.000000000000000000, 0.000000000000000000, -0.000000000000000000 ) ) ;
#13373 = CARTESIAN_POINT ( 'NONE',  ( 46.45491332379572924, 55.29948385550240175, -4.840751629271157874 ) ) ;
#13374 = DIRECTION ( 'NONE',  ( -0.000000000000000000, -0.000000000000000000, 1.000000000000000000 ) ) ;
#13375 = CARTESIAN_POINT ( 'NONE',  ( -1.575481281892997891E-16, 0.4887495715076908831, -5.000000000000000000 ) ) ;
#13376 = CARTESIAN_POINT ( 'NONE',  ( 56.79116909180259398, 51.20051614449766220, 4.963592699178938972 ) ) ;
#13377 = CARTESIAN_POINT ( 'NONE',  ( 44.91013252490150620, 52.20051614449766220, -3.727524721679154940 ) ) ;
#13378 = CIRCLE ( 'NONE', #4923, 4.999999999999999112 ) ;
#13379 = LINE ( 'NONE', #4567, #5998 ) ;
#13380 = AXIS2_PLACEMENT_3D ( 'NONE', #14770, #7327, #13302 ) ;
#13381 = CARTESIAN_POINT ( 'NONE',  ( -4.000000000000000000, 2.309401076758498483, -3.433295621305379353 ) ) ;
#13382 = ORIENTED_EDGE ( 'NONE', *, *, #11100, .T. ) ;
#13383 = ORIENTED_EDGE ( 'NONE', *, *, #1509, .T. ) ;
#13384 = DIRECTION ( 'NONE',  ( 0.000000000000000000, -0.000000000000000000, 1.000000000000000000 ) ) ;
#13385 = VERTEX_POINT ( 'NONE', #16077 ) ;
#13386 = EDGE_CURVE ( 'NONE', #10892, #8385, #15875, .T. ) ;
#13387 = CARTESIAN_POINT ( 'NONE',  ( 45.90387839640214196, 64.69948385550240744, 5.676469297603166098 ) ) ;
#13388 = CARTESIAN_POINT ( 'NONE',  ( -19.89043790736547379, -17.90943073464699609, -9.000000000000000000 ) ) ;
#13389 = EDGE_CURVE ( 'NONE', #6630, #14591, #8523, .T. ) ;
#13390 = AXIS2_PLACEMENT_3D ( 'NONE', #6295, #5394, #13138 ) ;
#13391 = ORIENTED_EDGE ( 'NONE', *, *, #1978, .T. ) ;
#13392 = DIRECTION ( 'NONE',  ( 0.000000000000000000, 0.000000000000000000, 1.000000000000000000 ) ) ;
#13393 = CARTESIAN_POINT ( 'NONE',  ( 50.02271294988512551, 46.49948385550240459, 7.000000000000000888 ) ) ;
#13394 = TOROIDAL_SURFACE ( 'NONE', #2776, 5.200000000000001066, 0.4999999999999978351 ) ;
#13395 = EDGE_CURVE ( 'NONE', #13559, #2940, #5572, .T. ) ;
#13396 = ORIENTED_EDGE ( 'NONE', *, *, #5083, .F. ) ;
#13397 = DIRECTION ( 'NONE',  ( 0.000000000000000000, 0.000000000000000000, -1.000000000000000000 ) ) ;
#13398 = EDGE_LOOP ( 'NONE', ( #18376, #19286, #3484, #12783 ) ) ;
#13399 = CARTESIAN_POINT ( 'NONE',  ( 56.79116909180255135, 45.79948385550240886, -4.963592699179005585 ) ) ;
#13400 = CARTESIAN_POINT ( 'NONE',  ( -10.75570504584948139, -3.819660112501066518, 9.000000000000000000 ) ) ;
#13401 = CARTESIAN_POINT ( 'NONE',  ( 57.36023556966787851, 59.99948385550240459, -0.02388180880522424582 ) ) ;
#13402 = CARTESIAN_POINT ( 'NONE',  ( -154.8605857259444463, -18.79744172571344762, 15.00000000000000000 ) ) ;
#13403 = CARTESIAN_POINT ( 'NONE',  ( 47.74827507625469281, 52.40051614449763662, -7.007379884777203749 ) ) ;
#13404 = CARTESIAN_POINT ( 'NONE',  ( 5.599999999999999645, -2.020725942163694722, -3.499999999999999556 ) ) ;
#13405 = CARTESIAN_POINT ( 'NONE',  ( 6.367873360227556567, 2.886751345948123770, -5.000000000000000000 ) ) ;
#13406 = CARTESIAN_POINT ( 'NONE',  ( -32.00000000000000000, -1.000000000000000000, -5.999999999999998224 ) ) ;
#13407 = EDGE_LOOP ( 'NONE', ( #358, #1896, #7787, #17628 ) ) ;
#13408 = CIRCLE ( 'NONE', #3095, 3.500000000000000000 ) ;
#13409 = EDGE_CURVE ( 'NONE', #9381, #6250, #17159, .T. ) ;
#13410 = AXIS2_PLACEMENT_3D ( 'NONE', #10190, #16190, #14705 ) ;
#13411 = ORIENTED_EDGE ( 'NONE', *, *, #18157, .F. ) ;
#13412 = APPLICATION_CONTEXT ( 'automotive_design' ) ;
#13413 = ORIENTED_EDGE ( 'NONE', *, *, #9069, .F. ) ;
#13414 = DIRECTION ( 'NONE',  ( -1.000000000000000000, 0.000000000000000000, 0.000000000000000000 ) ) ;
#13415 = EDGE_CURVE ( 'NONE', #11423, #14693, #18576, .T. ) ;
#13416 = CARTESIAN_POINT ( 'NONE',  ( 54.72065718078924590, 64.29948385550240175, 6.458785618021043895 ) ) ;
#13417 = DIRECTION ( 'NONE',  ( 0.9999419836444144449, 0.01077169184824073971, -2.272467923560868285E-17 ) ) ;
#13418 = EDGE_LOOP ( 'NONE', ( #1212, #17615, #9046, #13971 ) ) ;
#13419 = CARTESIAN_POINT ( 'NONE',  ( -4.154094228333736538, -2.398367420967545627, -3.721909803043222276 ) ) ;
#13420 = VERTEX_POINT ( 'NONE', #17453 ) ;
#13421 = CARTESIAN_POINT ( 'NONE',  ( 47.70284917648459810, 61.60051614449765367, 6.992620115222797139 ) ) ;
#13422 = EDGE_LOOP ( 'NONE', ( #17700, #19192, #19039, #8807 ) ) ;
#13423 = CIRCLE ( 'NONE', #909, 5.000000000000007994 ) ;
#13424 = CIRCLE ( 'NONE', #18771, 0.9999999999999993339 ) ;
#13425 = FACE_OUTER_BOUND ( 'NONE', #715, .T. ) ;
#13426 = PRODUCT_DEFINITION_CONTEXT ( 'detailed design', #9646, 'design' ) ;
#13427 = FACE_OUTER_BOUND ( 'NONE', #2599, .T. ) ;
#13428 = SHAPE_REPRESENTATION ( 'hex flange bolt small_iso_ISO 4162 - M8 x 45 x 22-N', ( #10359 ), #1541 ) ;
#13429 = CARTESIAN_POINT ( 'NONE',  ( 51.92680522751238925, 55.40051614449767214, 6.007379884777208190 ) ) ;
#13430 = DIRECTION ( 'NONE',  ( 0.000000000000000000, 0.000000000000000000, -1.000000000000000000 ) ) ;
#13431 =( LENGTH_UNIT ( ) NAMED_UNIT ( * ) SI_UNIT ( .MILLI., .METRE. ) );
#13432 = CARTESIAN_POINT ( 'NONE',  ( 48.02776887271745210, 59.39948385550240317, -5.992620115222778487 ) ) ;
#13433 = CARTESIAN_POINT ( 'NONE',  ( -0.1404048886732797152, -4.699864953788083888, -3.686887068327043160 ) ) ;
#13434 = CARTESIAN_POINT ( 'NONE',  ( 43.33558569842703179, 51.09948385550240602, -2.141517661632099223 ) ) ;
#13435 = CARTESIAN_POINT ( 'NONE',  ( 54.68390685589039890, 53.30051614449767072, 6.485486291978072693 ) ) ;
#13436 = FACE_OUTER_BOUND ( 'NONE', #9926, .T. ) ;
#13437 = CARTESIAN_POINT ( 'NONE',  ( 3.948103430091020272, 2.682758828852976229, -2.353325403973173024 ) ) ;
#13438 = CARTESIAN_POINT ( 'NONE',  ( -0.9999999999999976685, -20.00000000000000000, -9.000000000000001776 ) ) ;
#13439 = SURFACE_STYLE_FILL_AREA ( #2963 ) ;
#13440 = VECTOR ( 'NONE', #10218, 1000.000000000000000 ) ;
#13441 = CIRCLE ( 'NONE', #9998, 20.00000000000000000 ) ;
#13442 = APPLICATION_PROTOCOL_DEFINITION ( 'draft international standard', 'automotive_design', 1998, #9646 ) ;
#13443 = EDGE_LOOP ( 'NONE', ( #4976, #14588, #2017, #8528, #2666 ) ) ;
#13444 = DIRECTION ( 'NONE',  ( -0.000000000000000000, -0.000000000000000000, -1.000000000000000000 ) ) ;
#13445 = CARTESIAN_POINT ( 'NONE',  ( 0.000000000000000000, -0.8865213383406730374, -1.535499999999999421 ) ) ;
#13446 = CARTESIAN_POINT ( 'NONE',  ( 45.90387839640214196, 62.69948385550240744, 5.676469297603166098 ) ) ;
#13447 = CARTESIAN_POINT ( 'NONE',  ( -74.99999999999997158, 32.50000000000001421, 15.00000000000000000 ) ) ;
#13448 = VECTOR ( 'NONE', #9429, 1000.000000000000000 ) ;
#13449 = DIRECTION ( 'NONE',  ( 0.000000000000000000, 0.000000000000000000, -1.000000000000000000 ) ) ;
#13450 = PLANE ( 'NONE',  #4007 ) ;
#13451 = CARTESIAN_POINT ( 'NONE',  ( 47.70284917648453415, 57.39948385550241028, -6.992620115222774047 ) ) ;
#13452 = LINE ( 'NONE', #8847, #3197 ) ;
#13453 = CARTESIAN_POINT ( 'NONE',  ( 57.61547081786812896, 56.09948385550240602, 2.450534656007040901 ) ) ;
#13454 = CARTESIAN_POINT ( 'NONE',  ( 4.052424581287701777, -3.786734753435149425, -0.5771415817957858962 ) ) ;
#13455 = EDGE_CURVE ( 'NONE', #17828, #17145, #14192, .T. ) ;
#13456 = CARTESIAN_POINT ( 'NONE',  ( 47.70284917648459100, 53.60051614449765367, 6.992620115222796251 ) ) ;
#13457 = AXIS2_PLACEMENT_3D ( 'NONE', #2492, #12765, #18764 ) ;
#13458 = DIRECTION ( 'NONE',  ( -1.000000000000000000, 0.000000000000000000, 0.000000000000000000 ) ) ;
#13459 = ADVANCED_FACE ( 'NONE', ( #871 ), #2563, .T. ) ;
#13460 = ORIENTED_EDGE ( 'NONE', *, *, #16975, .T. ) ;
#13461 = EDGE_CURVE ( 'NONE', #17357, #13102, #9022, .T. ) ;
#13462 =( NAMED_UNIT ( * ) SI_UNIT ( $, .STERADIAN. ) SOLID_ANGLE_UNIT ( ) );
#13463 = EDGE_LOOP ( 'NONE', ( #282, #13707 ) ) ;
#13464 = ADVANCED_FACE ( 'NONE', ( #17552 ), #10079, .F. ) ;
#13465 = ADVANCED_FACE ( 'NONE', ( #15684 ), #7921, .F. ) ;
#13466 = DIRECTION ( 'NONE',  ( -0.000000000000000000, -0.000000000000000000, 1.000000000000000000 ) ) ;
#13467 = ORIENTED_EDGE ( 'NONE', *, *, #6096, .T. ) ;
#13468 = CARTESIAN_POINT ( 'NONE',  ( 6.367873360227558344, 5.773502691896261751, 0.000000000000000000 ) ) ;
#13469 = EDGE_CURVE ( 'NONE', #3609, #5700, #19075, .T. ) ;
#13470 = ORIENTED_EDGE ( 'NONE', *, *, #6290, .T. ) ;
#13471 = CIRCLE ( 'NONE', #4709, 1.000000000000000888 ) ;
#13472 = CARTESIAN_POINT ( 'NONE',  ( 1.249999999999997558, 0.000000000000000000, 0.000000000000000000 ) ) ;
#13473 = ORIENTED_EDGE ( 'NONE', *, *, #12858, .T. ) ;
#13474 = CARTESIAN_POINT ( 'NONE',  ( -62.49999999999997158, 45.00000000000001421, 15.00000000000000000 ) ) ;
#13475 = DIRECTION ( 'NONE',  ( 0.000000000000000000, 1.000000000000000000, 0.000000000000000000 ) ) ;
#13476 = CARTESIAN_POINT ( 'NONE',  ( 43.69122665457040000, 58.99948385550239749, 0.02388180880521036456 ) ) ;
#13477 = DIRECTION ( 'NONE',  ( 0.000000000000000000, 0.000000000000000000, 1.000000000000000000 ) ) ;
#13478 = CARTESIAN_POINT ( 'NONE',  ( 43.20883090819742023, 54.20051614449766220, -4.963592699178938972 ) ) ;
#13479 = AXIS2_PLACEMENT_3D ( 'NONE', #6138, #3117, #1249 ) ;
#13480 = EDGE_CURVE ( 'NONE', #13933, #13007, #15010, .T. ) ;
#13481 = CARTESIAN_POINT ( 'NONE',  ( 51.97223112728249816, 58.60051614449766788, -5.992620115222793586 ) ) ;
#13482 = ADVANCED_FACE ( 'NONE', ( #1362 ), #7335, .F. ) ;
#13484 = CIRCLE ( 'NONE', #8774, 1.000000000000001110 ) ;
#13483 = CARTESIAN_POINT ( 'NONE',  ( -154.9999999999999716, -14.99999999999999645, -10.00000000000000178 ) ) ;
#13485 = AXIS2_PLACEMENT_3D ( 'NONE', #16643, #18116, #12012 ) ;
#13486 = FACE_OUTER_BOUND ( 'NONE', #18304, .T. ) ;
#13487 = ORIENTED_EDGE ( 'NONE', *, *, #6518, .F. ) ;
#13488 = CIRCLE ( 'NONE', #14414, 2.649999999999985700 ) ;
#13489 = VERTEX_POINT ( 'NONE', #8994 ) ;
#13490 = DIRECTION ( 'NONE',  ( 0.000000000000000000, 0.000000000000000000, -1.000000000000000000 ) ) ;
#13491 = VERTEX_POINT ( 'NONE', #10371 ) ;
#13492 = CARTESIAN_POINT ( 'NONE',  ( 50.02271294988512551, 64.49948385550240459, 7.000000000000000888 ) ) ;
#13493 = FACE_OUTER_BOUND ( 'NONE', #6824, .T. ) ;
#13494 = ORIENTED_EDGE ( 'NONE', *, *, #6221, .F. ) ;
#13495 = DIRECTION ( 'NONE',  ( -1.000000000000000000, 0.000000000000000000, 0.000000000000000000 ) ) ;
#13496 = AXIS2_PLACEMENT_3D ( 'NONE', #15182, #7824, #7730 ) ;
#13497 = DIRECTION ( 'NONE',  ( 1.000000000000000000, 0.000000000000000000, 0.000000000000000000 ) ) ;
#13498 = ORIENTED_EDGE ( 'NONE', *, *, #10577, .T. ) ;
#13499 = CARTESIAN_POINT ( 'NONE',  ( -7.134732861516020819, -1.729090847147989773, -9.000000000000000000 ) ) ;
#13500 = AXIS2_PLACEMENT_3D ( 'NONE', #15128, #135, #10318 ) ;
#13501 = ORIENTED_EDGE ( 'NONE', *, *, #1486, .T. ) ;
#13502 = CARTESIAN_POINT ( 'NONE',  ( 52.57664461997811856, 45.59948385550240602, -8.007379884777229506 ) ) ;
#13503 = AXIS2_PLACEMENT_3D ( 'NONE', #17401, #12877, #2305 ) ;
#13504 = CARTESIAN_POINT ( 'NONE',  ( 54.23491683972284960, 45.00000000000001421, -4.999999999999999112 ) ) ;
#13505 = CARTESIAN_POINT ( 'NONE',  ( 45.86712807150323812, 55.29948385550240175, -5.649768623646098220 ) ) ;
#13506 = CARTESIAN_POINT ( 'NONE',  ( 6.445379721942638973, 2.463581311471617852, 5.110653333236676588 ) ) ;
#13507 = CARTESIAN_POINT ( 'NONE',  ( 30.00000000000000000, -7.499999999999971578, -10.00000000000000000 ) ) ;
#13508 = CARTESIAN_POINT ( 'NONE',  ( 43.33558569842706021, 51.90051614449765793, 2.141517661632167169 ) ) ;
#13509 = DIRECTION ( 'NONE',  ( -0.000000000000000000, -0.000000000000000000, -1.000000000000000000 ) ) ;
#13510 = LINE ( 'NONE', #14971, #3200 ) ;
#13511 = CARTESIAN_POINT ( 'NONE',  ( -4.211399284164270895, 2.459729995988205964, -3.751162237960538715 ) ) ;
#13512 = VERTEX_POINT ( 'NONE', #11940 ) ;
#13513 = AXIS2_PLACEMENT_3D ( 'NONE', #4951, #10924, #736 ) ;
#13514 = EDGE_LOOP ( 'NONE', ( #14344, #17654, #16749, #15812 ) ) ;
#13515 = ORIENTED_EDGE ( 'NONE', *, *, #18887, .F. ) ;
#13516 = DIRECTION ( 'NONE',  ( 0.000000000000000000, 0.000000000000000000, 1.000000000000000000 ) ) ;
#13517 =( LENGTH_UNIT ( ) NAMED_UNIT ( * ) SI_UNIT ( .MILLI., .METRE. ) );
#13518 = CARTESIAN_POINT ( 'NONE',  ( 54.13287192849676188, 46.29948385550240886, 5.649768623646098220 ) ) ;
#13519 = AXIS2_PLACEMENT_3D ( 'NONE', #9365, #6524, #7281 ) ;
#13520 = FACE_OUTER_BOUND ( 'NONE', #4594, .T. ) ;
#13521 = EDGE_LOOP ( 'NONE', ( #16213, #11697 ) ) ;
#13522 = CARTESIAN_POINT ( 'NONE',  ( 6.534533895392296010, 5.902695350657467088, 5.075181882648644095E-15 ) ) ;
#13523 = EDGE_LOOP ( 'NONE', ( #6334, #5541, #14855, #352 ) ) ;
#13524 = CARTESIAN_POINT ( 'NONE',  ( 43.33558569842706021, 61.90051614449766504, 2.141517661632167169 ) ) ;
#13525 = ORIENTED_EDGE ( 'NONE', *, *, #5683, .F. ) ;
#13526 = EDGE_CURVE ( 'NONE', #7511, #2842, #5972, .T. ) ;
#13527 = DIRECTION ( 'NONE',  ( -1.000000000000000000, 0.000000000000000000, 0.000000000000000000 ) ) ;
#13528 = DIRECTION ( 'NONE',  ( -1.000000000000000000, 0.000000000000000000, 0.000000000000000000 ) ) ;
#13529 = CARTESIAN_POINT ( 'NONE',  ( 48.02776887271750184, 55.60051614449765367, 5.992620115222795363 ) ) ;
#13530 = DIRECTION ( 'NONE',  ( 1.000000000000000000, 0.000000000000000000, 0.000000000000000000 ) ) ;
#13531 = EDGE_CURVE ( 'NONE', #10950, #7334, #8717, .T. ) ;
#13532 = CARTESIAN_POINT ( 'NONE',  ( -32.00000000000000000, 1.000000000000000000, 6.000000000000000000 ) ) ;
#13533 = AXIS2_PLACEMENT_3D ( 'NONE', #10356, #1155, #8229 ) ;
#13534 = CARTESIAN_POINT ( 'NONE',  ( 43.69122665457040000, 56.99948385550241170, 0.02388180880521036456 ) ) ;
#13535 = LINE ( 'NONE', #14998, #4439 ) ;
#13536 = CARTESIAN_POINT ( 'NONE',  ( 42.38452918213190657, 53.90051614449765793, 2.450534656007115508 ) ) ;
#13537 = CARTESIAN_POINT ( 'NONE',  ( 6.507056315241511513, -2.833450876375909644, 5.092319121366346124 ) ) ;
#13538 = CARTESIAN_POINT ( 'NONE',  ( 2.449293598294706513E-15, -20.00000000000000000, 9.000000000000000000 ) ) ;
#13539 = EDGE_LOOP ( 'NONE', ( #10843, #5673, #16170, #13206, #3303, #16511, #10148, #9333 ) ) ;
#13540 = CARTESIAN_POINT ( 'NONE',  ( 2.449293598294706513E-15, -20.00000000000000000, 9.000000000000000000 ) ) ;
#13541 = APPLICATION_PROTOCOL_DEFINITION ( 'draft international standard', 'automotive_design', 1998, #7285 ) ;
#13542 = CIRCLE ( 'NONE', #17629, 2.396904916527699214 ) ;
#13543 = ORIENTED_EDGE ( 'NONE', *, *, #8673, .F. ) ;
#13544 = DIRECTION ( 'NONE',  ( 1.000000000000000000, 0.000000000000000000, 0.000000000000000000 ) ) ;
#13545 = DIRECTION ( 'NONE',  ( -0.7779254092217071648, -0.6283566325640553840, 0.000000000000000000 ) ) ;
#13546 = CARTESIAN_POINT ( 'NONE',  ( 45.86712807150323812, 65.29948385550241596, -5.649768623646098220 ) ) ;
#13547 = CARTESIAN_POINT ( 'NONE',  ( 6.506987859255518813, 2.925375531177291766, 5.066899051217865768 ) ) ;
#13548 = DIRECTION ( 'NONE',  ( 0.000000000000000000, 0.000000000000000000, -1.000000000000000000 ) ) ;
#13549 = CARTESIAN_POINT ( 'NONE',  ( -20.00000000000000000, -19.99999999999999289, -20.00000000000000000 ) ) ;
#13550 = CARTESIAN_POINT ( 'NONE',  ( 44.05948171654949874, 60.79948385550240886, 4.345558710429105354 ) ) ;
#13551 = DIRECTION ( 'NONE',  ( 0.000000000000000000, 0.000000000000000000, 1.000000000000000000 ) ) ;
#13552 = CARTESIAN_POINT ( 'NONE',  ( 43.20883090819745576, 50.79948385550240175, 4.963592699179006473 ) ) ;
#13553 = CARTESIAN_POINT ( 'NONE',  ( 4.180231891692620216, -2.049421325483211653, -3.591231015387276848 ) ) ;
#13554 = CARTESIAN_POINT ( 'NONE',  ( 45.86712807150329496, 51.70051614449766220, 5.649768623646139964 ) ) ;
#13555 = PRODUCT_DEFINITION_FORMATION_WITH_SPECIFIED_SOURCE ( 'ANY', '', #4453, .NOT_KNOWN. ) ;
#13556 = FACE_BOUND ( 'NONE', #9933, .T. ) ;
#13557 = ORIENTED_EDGE ( 'NONE', *, *, #16593, .F. ) ;
#13558 =( NAMED_UNIT ( * ) SI_UNIT ( $, .STERADIAN. ) SOLID_ANGLE_UNIT ( ) );
#13559 = VERTEX_POINT ( 'NONE', #14978 ) ;
#13560 = CARTESIAN_POINT ( 'NONE',  ( 1.567478505476134606E-15, 4.618802153517012066, -3.433295621305382905 ) ) ;
#13561 = ORIENTED_EDGE ( 'NONE', *, *, #12496, .T. ) ;
#13562 = DIRECTION ( 'NONE',  ( -1.000000000000000000, 0.000000000000000000, 0.000000000000000000 ) ) ;
#13563 = EDGE_CURVE ( 'NONE', #730, #5970, #4659, .T. ) ;
#13564 = CARTESIAN_POINT ( 'NONE',  ( 53.50000000000000000, 0.000000000000000000, 0.000000000000000000 ) ) ;
#13565 = CARTESIAN_POINT ( 'NONE',  ( 1.317756351988342622, -3.857995168970215438, -0.04852650426602527628 ) ) ;
#13566 = ORIENTED_EDGE ( 'NONE', *, *, #2274, .F. ) ;
#13567 = LINE ( 'NONE', #18095, #13968 ) ;
#13568 = CARTESIAN_POINT ( 'NONE',  ( 2.000000000000000000, 2.065682573263594481E-15, 1.535500000000000309 ) ) ;
#13569 = CARTESIAN_POINT ( 'NONE',  ( 55.08986747509847248, 57.79948385550240175, -3.727524721679197572 ) ) ;
#13570 = DIRECTION ( 'NONE',  ( 0.000000000000000000, 0.000000000000000000, 1.000000000000000000 ) ) ;
#13571 = CARTESIAN_POINT ( 'NONE',  ( 52.62207051974829852, 52.60051614449765367, -7.992620115222797139 ) ) ;
#13572 = CARTESIAN_POINT ( 'NONE',  ( 44.88205777487401349, 53.80051614449766362, 3.688883143319584779 ) ) ;
#13573 = CARTESIAN_POINT ( 'NONE',  ( 62.49999999999998579, 45.00000000000001421, 15.00000000000000000 ) ) ;
#13574 = DIRECTION ( 'NONE',  ( -0.000000000000000000, -0.000000000000000000, -1.000000000000000000 ) ) ;
#13575 = ORIENTED_EDGE ( 'NONE', *, *, #5909, .T. ) ;
#13576 = EDGE_CURVE ( 'NONE', #16928, #2243, #1227, .T. ) ;
#13577 = ORIENTED_EDGE ( 'NONE', *, *, #2409, .T. ) ;
#13578 = CARTESIAN_POINT ( 'NONE',  ( 54.23491683972284960, 45.00000000000001421, -4.999999999999999112 ) ) ;
#13579 = VERTEX_POINT ( 'NONE', #10266 ) ;
#13580 = CARTESIAN_POINT ( 'NONE',  ( 42.63976443033212860, 62.99948385550241170, 0.02388180880522514787 ) ) ;
#13581 = CARTESIAN_POINT ( 'NONE',  ( 3.973514160553462737, -3.435084588004193140, 1.181876024140318782 ) ) ;
#13582 = ORIENTED_EDGE ( 'NONE', *, *, #19236, .T. ) ;
#13583 = DIRECTION ( 'NONE',  ( -1.000000000000000000, 0.000000000000000000, 0.000000000000000000 ) ) ;
#13584 = EDGE_CURVE ( 'NONE', #4647, #3704, #10555, .T. ) ;
#13585 = FACE_OUTER_BOUND ( 'NONE', #6226, .T. ) ;
#13586 = ADVANCED_FACE ( 'NONE', ( #16562 ), #14880, .T. ) ;
#13587 = ORIENTED_EDGE ( 'NONE', *, *, #5694, .T. ) ;
#13588 = LINE ( 'NONE', #3215, #5363 ) ;
#13589 = ORIENTED_EDGE ( 'NONE', *, *, #6644, .F. ) ;
#13590 = CARTESIAN_POINT ( 'NONE',  ( 41.58830220609386430, 64.00051614449765225, -0.02388180880514929535 ) ) ;
#13591 = AXIS2_PLACEMENT_3D ( 'NONE', #1790, #13551, #16407 ) ;
#13592 = CARTESIAN_POINT ( 'NONE',  ( 30.00000000000000355, -39.99999999999998579, -10.00000000000000178 ) ) ;
#13593 = CARTESIAN_POINT ( 'NONE',  ( 54.13287192849676188, 56.29948385550240175, 5.649768623646098220 ) ) ;
#13594 = CARTESIAN_POINT ( 'NONE',  ( 1.925929944387235853E-31, 15.00000000000001599, -15.00000000000000000 ) ) ;
#13595 = CARTESIAN_POINT ( 'NONE',  ( -0.1717365941144614327, -6.008326913195983998, -0.8000000000000000444 ) ) ;
#13596 = CARTESIAN_POINT ( 'NONE',  ( 54.09612160359792199, 51.30051614449766362, 5.676469297603124353 ) ) ;
#13597 = DIRECTION ( 'NONE',  ( 1.000000000000000000, 0.000000000000000000, 0.000000000000000000 ) ) ;
#13598 = EDGE_CURVE ( 'NONE', #16565, #7129, #15085, .T. ) ;
#13599 = DIRECTION ( 'NONE',  ( -1.000000000000000000, 0.000000000000000000, 0.000000000000000000 ) ) ;
#13600 = PLANE ( 'NONE',  #12219 ) ;
#13601 = ORIENTED_EDGE ( 'NONE', *, *, #3413, .F. ) ;
#13602 = ORIENTED_EDGE ( 'NONE', *, *, #13584, .F. ) ;
#13603 = ORIENTED_EDGE ( 'NONE', *, *, #82, .F. ) ;
#13604 = CARTESIAN_POINT ( 'NONE',  ( -99.99999999999997158, -6.999999999999992895, 15.00000000000000000 ) ) ;
#13605 = VECTOR ( 'NONE', #2578, 1000.000000000000000 ) ;
#13606 = CARTESIAN_POINT ( 'NONE',  ( 42.38452918213188525, 63.09948385550240602, -2.450534656007040013 ) ) ;
#13607 = DIRECTION ( 'NONE',  ( -1.000000000000000000, 0.000000000000000000, 0.000000000000000000 ) ) ;
#13608 = ORIENTED_EDGE ( 'NONE', *, *, #9442, .T. ) ;
#13609 = LINE ( 'NONE', #18141, #17105 ) ;
#13610 = EDGE_CURVE ( 'NONE', #9852, #14377, #17652, .T. ) ;
#13611 = ORIENTED_EDGE ( 'NONE', *, *, #17341, .F. ) ;
#13612 = CARTESIAN_POINT ( 'NONE',  ( 44.03140696652198471, 59.80051614449766362, 4.306917132069485454 ) ) ;
#13613 = ORIENTED_EDGE ( 'NONE', *, *, #10584, .F. ) ;
#13614 = LINE ( 'NONE', #14990, #16629 ) ;
#13615 = UNCERTAINTY_MEASURE_WITH_UNIT (LENGTH_MEASURE( 1.000000000000000082E-05 ), #10846, 'distance_accuracy_value', 'NONE');
#13616 = LINE ( 'NONE', #18342, #18723 ) ;
#13617 = AXIS2_PLACEMENT_3D ( 'NONE', #3731, #5391, #11362 ) ;
#13618 = AXIS2_PLACEMENT_3D ( 'NONE', #16070, #15869, #11442 ) ;
#13619 = CARTESIAN_POINT ( 'NONE',  ( 44.88205777487401349, 53.80051614449766362, 3.688883143319584779 ) ) ;
#13620 = DIRECTION ( 'NONE',  ( 0.000000000000000000, 0.000000000000000000, 1.000000000000000000 ) ) ;
#13621 = CARTESIAN_POINT ( 'NONE',  ( -54.99999999999996447, -22.99999999999998579, -15.00000000000000000 ) ) ;
#13622 = CARTESIAN_POINT ( 'NONE',  ( 51.92680522751233951, 59.59948385550240602, -6.007379884777223289 ) ) ;
#13623 = DIRECTION ( 'NONE',  ( 1.000000000000000000, 0.000000000000000000, 0.000000000000000000 ) ) ;
#13624 = AXIS2_PLACEMENT_3D ( 'NONE', #11191, #9723, #3661 ) ;
#13625 = CARTESIAN_POINT ( 'NONE',  ( 54.72065718078918906, 52.70051614449766220, -6.458785618021089192 ) ) ;
#13626 = LINE ( 'NONE', #18158, #19124 ) ;
#13627 = CARTESIAN_POINT ( 'NONE',  ( 3.951447005078453589, -3.704664227300103807, 0.5833333333333329263 ) ) ;
#13628 = ORIENTED_EDGE ( 'NONE', *, *, #5099, .F. ) ;
#13629 = DIRECTION ( 'NONE',  ( 0.000000000000000000, 0.000000000000000000, 1.000000000000000000 ) ) ;
#13630 = ADVANCED_FACE ( 'NONE', ( #2751, #8707, #16269, #14685 ), #1267, .T. ) ;
#13631 = PRODUCT_CONTEXT ( 'NONE', #17284, 'mechanical' ) ;
#13632 = VERTEX_POINT ( 'NONE', #5770 ) ;
#13633 = DIRECTION ( 'NONE',  ( -1.000000000000000000, -0.000000000000000000, -0.000000000000000000 ) ) ;
#13634 = EDGE_CURVE ( 'NONE', #2509, #5072, #9855, .T. ) ;
#13635 = DIRECTION ( 'NONE',  ( 0.000000000000000000, 0.000000000000000000, -1.000000000000000000 ) ) ;
#13636 = AXIS2_PLACEMENT_3D ( 'NONE', #2465, #19037, #4307 ) ;
#13637 = CARTESIAN_POINT ( 'NONE',  ( 43.33558569842703179, 61.09948385550240602, -2.141517661632099223 ) ) ;
#13638 = CARTESIAN_POINT ( 'NONE',  ( -154.9999999999999716, -14.99999999999999645, -3.999999999999999112 ) ) ;
#13639 = CARTESIAN_POINT ( 'NONE',  ( -99.99999999999997158, -6.999999999999992895, 10.00000000000000000 ) ) ;
#13640 = CARTESIAN_POINT ( 'NONE',  ( 2.449293598294706513E-15, -20.00000000000000000, 9.000000000000000000 ) ) ;
#13641 = CIRCLE ( 'NONE', #15513, 7.500000000000000888 ) ;
#13642 = CARTESIAN_POINT ( 'NONE',  ( 50.02271294988512551, 58.49948385550241170, 7.000000000000000888 ) ) ;
#13643 = CARTESIAN_POINT ( 'NONE',  ( 3.309651814758564736, -5.455921364805393026, -1.000000000000000000 ) ) ;
#13644 = CARTESIAN_POINT ( 'NONE',  ( 43.18075615816989199, 55.19948385550240744, -4.924951120819313743 ) ) ;
#13645 = CARTESIAN_POINT ( 'NONE',  ( 6.534838248920900483, -5.903531555104836848, 4.671345613696493211E-16 ) ) ;
#13646 = CARTESIAN_POINT ( 'NONE',  ( 57.36023556966787851, 53.00051614449765225, 0.02388180880515038476 ) ) ;
#13647 = CARTESIAN_POINT ( 'NONE',  ( -154.9999999999999716, -14.99999999999999645, -9.000000000000000000 ) ) ;
#13648 = AXIS2_PLACEMENT_3D ( 'NONE', #6731, #3418, #12715 ) ;
#13649 = ADVANCED_FACE ( 'NONE', ( #1457 ), #10459, .F. ) ;
#13650 =( NAMED_UNIT ( * ) SI_UNIT ( $, .STERADIAN. ) SOLID_ANGLE_UNIT ( ) );
#13651 = ORIENTED_EDGE ( 'NONE', *, *, #13710, .T. ) ;
#13652 = COLOUR_RGB ( '',0.8941176470588234615, 0.8941176470588234615, 0.8941176470588234615 ) ;
#13653 = CARTESIAN_POINT ( 'NONE',  ( 6.534533895392294234, 2.951347675328729991, -5.111884124469655788 ) ) ;
#13654 = EDGE_LOOP ( 'NONE', ( #7789, #9105 ) ) ;
#13655 = CARTESIAN_POINT ( 'NONE',  ( 56.66441430157294690, 48.90051614449766504, -2.141517661632166281 ) ) ;
#13656 = CARTESIAN_POINT ( 'NONE',  ( 50.02271294988512551, 64.49948385550240459, 7.000000000000000888 ) ) ;
#13657 = CARTESIAN_POINT ( 'NONE',  ( 2.449293598294706513E-15, -20.00000000000000000, 9.000000000000000000 ) ) ;
#13658 = ORIENTED_EDGE ( 'NONE', *, *, #1869, .F. ) ;
#13659 = DIRECTION ( 'NONE',  ( -0.000000000000000000, 0.000000000000000000, -1.000000000000000000 ) ) ;
#13660 = DIRECTION ( 'NONE',  ( 1.000000000000000000, 0.000000000000000000, 0.000000000000000000 ) ) ;
#13661 = CARTESIAN_POINT ( 'NONE',  ( 55.71335778527780747, 58.09948385550241312, 1.832500667257165983 ) ) ;
#13662 = CARTESIAN_POINT ( 'NONE',  ( -29.99999999999999645, 40.00000000000000000, 10.00000000000000000 ) ) ;
#13663 =( REPRESENTATION_RELATIONSHIP ('NONE','NONE', #16703, #18081 ) REPRESENTATION_RELATIONSHIP_WITH_TRANSFORMATION ( #5096 )SHAPE_REPRESENTATION_RELATIONSHIP( ) );
#13664 = CARTESIAN_POINT ( 'NONE',  ( 41.58830220609386430, 54.00051614449765935, -0.02388180880514929535 ) ) ;
#13665 = CARTESIAN_POINT ( 'NONE',  ( 44.91013252490150620, 56.20051614449766220, -3.727524721679154940 ) ) ;
#13666 = CARTESIAN_POINT ( 'NONE',  ( 1.250000000000001110, 0.000000000000000000, 0.000000000000000000 ) ) ;
#13667 = CARTESIAN_POINT ( 'NONE',  ( -179.9999999999999716, -15.00000000000000000, -3.999999999999999112 ) ) ;
#13668 = ORIENTED_EDGE ( 'NONE', *, *, #16344, .F. ) ;
#13669 = VECTOR ( 'NONE', #14026, 1000.000000000000000 ) ;
#13670 = VERTEX_POINT ( 'NONE', #9371 ) ;
#13671 = DIRECTION ( 'NONE',  ( -1.000000000000000000, -0.000000000000000000, -0.000000000000000000 ) ) ;
#13672 = VERTEX_POINT ( 'NONE', #559 ) ;
#13673 = LINE ( 'NONE', #5046, #1236 ) ;
#13674 = EDGE_LOOP ( 'NONE', ( #65, #13487 ) ) ;
#13675 = CARTESIAN_POINT ( 'NONE',  ( -20.00000000000000000, -19.99999999999999289, -20.00000000000000000 ) ) ;
#13676 = CARTESIAN_POINT ( 'NONE',  ( 49.97728705011488159, 51.49948385550240459, -7.000000000000000888 ) ) ;
#13677 = VECTOR ( 'NONE', #15164, 1000.000000000000000 ) ;
#13678 = ORIENTED_EDGE ( 'NONE', *, *, #5446, .T. ) ;
#13679 = LINE ( 'NONE', #4487, #5052 ) ;
#13680 = ORIENTED_EDGE ( 'NONE', *, *, #50, .T. ) ;
#13681 = CARTESIAN_POINT ( 'NONE',  ( 54.68390685589033495, 45.69948385550240033, -6.485486291978119766 ) ) ;
#13682 = CARTESIAN_POINT ( 'NONE',  ( 2.344047193898588954, 3.265465875126468021, -5.031375706690542042E-16 ) ) ;
#13683 = AXIS2_PLACEMENT_3D ( 'NONE', #6782, #9909, #11381 ) ;
#13684 = CARTESIAN_POINT ( 'NONE',  ( 47.70284917648453415, 59.39948385550241028, -6.992620115222774047 ) ) ;
#13685 = CARTESIAN_POINT ( 'NONE',  ( 62.49999999999998579, 5.000000000000018652, -5.000000000000000000 ) ) ;
#13686 = LINE ( 'NONE', #18230, #243 ) ;
#13687 = VECTOR ( 'NONE', #7825, 1000.000000000000000 ) ;
#13688 = CARTESIAN_POINT ( 'NONE',  ( 55.94051828345053679, 55.20051614449766930, 4.345558710429044069 ) ) ;
#13689 = DIRECTION ( 'NONE',  ( 0.000000000000000000, 0.000000000000000000, 1.000000000000000000 ) ) ;
#13690 = CARTESIAN_POINT ( 'NONE',  ( 6.534838248920900483, -5.903531555104836848, 4.671345613696493211E-16 ) ) ;
#13691 = ORIENTED_EDGE ( 'NONE', *, *, #5191, .T. ) ;
#13692 = EDGE_CURVE ( 'NONE', #3574, #11631, #2039, .T. ) ;
#13693 = ORIENTED_EDGE ( 'NONE', *, *, #4188, .T. ) ;
#13694 = CIRCLE ( 'NONE', #12446, 1.610000000000000098 ) ;
#13695 = ORIENTED_EDGE ( 'NONE', *, *, #14355, .T. ) ;
#13696 = DIRECTION ( 'NONE',  ( -1.000000000000000000, -0.000000000000000000, -0.000000000000000000 ) ) ;
#13697 = PRODUCT_RELATED_PRODUCT_CATEGORY ( 'part', '', ( #16350 ) ) ;
#13698 = ADVANCED_FACE ( 'NONE', ( #4791 ), #17510, .T. ) ;
#13699 = CONICAL_SURFACE ( 'NONE', #16837, 3.500000000000000000, 1.047197551196600296 ) ;
#13700 = CARTESIAN_POINT ( 'NONE',  ( 47.42335538002188144, 62.59948385550238470, 8.007379884777233059 ) ) ;
#13701 = CARTESIAN_POINT ( 'NONE',  ( 15.51323935927256237, -7.377028694403341191, -9.000000000000000000 ) ) ;
#13702 = EDGE_LOOP ( 'NONE', ( #12252, #3016, #17023, #14636 ) ) ;
#13703 = AXIS2_PLACEMENT_3D ( 'NONE', #4079, #5740, #10045 ) ;
#13704 = CARTESIAN_POINT ( 'NONE',  ( -4.024497503033519941, -2.323544716729390558, -3.572167766733381544 ) ) ;
#13705 = EDGE_CURVE ( 'NONE', #402, #3962, #16850, .T. ) ;
#13706 = EDGE_CURVE ( 'NONE', #2011, #4060, #2485, .T. ) ;
#13707 = ORIENTED_EDGE ( 'NONE', *, *, #14474, .F. ) ;
#13708 = CARTESIAN_POINT ( 'NONE',  ( 55.94051828345054389, 57.20051614449766220, 4.345558710429044957 ) ) ;
#13709 = ORIENTED_EDGE ( 'NONE', *, *, #5617, .F. ) ;
#13710 = EDGE_CURVE ( 'NONE', #6135, #1616, #7790, .T. ) ;
#13711 = CARTESIAN_POINT ( 'NONE',  ( 5.100000000000002309, 0.000000000000000000, 0.000000000000000000 ) ) ;
#13712 = DIRECTION ( 'NONE',  ( -1.000000000000000000, -0.000000000000000000, -0.000000000000000000 ) ) ;
#13713 = CARTESIAN_POINT ( 'NONE',  ( 53.54508667620424234, 56.70051614449766930, -4.840751629271188961 ) ) ;
#13714 = CARTESIAN_POINT ( 'NONE',  ( -154.9999999999999716, -14.99999999999999645, -15.00000000000000000 ) ) ;
#13715 = AXIS2_PLACEMENT_3D ( 'NONE', #5701, #11273, #9897 ) ;
#13716 = SURFACE_STYLE_USAGE ( .BOTH. , #576 ) ;
#13717 = CARTESIAN_POINT ( 'NONE',  ( 46.45491332379572924, 65.29948385550241596, -4.840751629271157874 ) ) ;
#13718 = CARTESIAN_POINT ( 'NONE',  ( -2.141980652367355020, -6.189445006155633422, -0.8000000000000000444 ) ) ;
#13719 = EDGE_CURVE ( 'NONE', #18444, #6580, #13424, .T. ) ;
#13720 = CARTESIAN_POINT ( 'NONE',  ( 54.68390685589039890, 55.30051614449765651, 6.485486291978072693 ) ) ;
#13721 = CARTESIAN_POINT ( 'NONE',  ( 1.000000000000002442, -20.00000000000000000, 8.999999999999998224 ) ) ;
#13722 = EDGE_CURVE ( 'NONE', #16015, #3393, #4966, .T. ) ;
#13723 = ORIENTED_EDGE ( 'NONE', *, *, #4373, .T. ) ;
#13724 = CARTESIAN_POINT ( 'NONE',  ( 2.354826896168714434, -6.962563485461402024, -1.000000000000000000 ) ) ;
#13725 = ORIENTED_EDGE ( 'NONE', *, *, #11667, .T. ) ;
#13726 = PRODUCT_CONTEXT ( 'NONE', #14889, 'mechanical' ) ;
#13727 = ORIENTED_EDGE ( 'NONE', *, *, #19004, .F. ) ;
#13728 = CARTESIAN_POINT ( 'NONE',  ( -4.999999999999998224, -20.00000000000000000, 15.00000000000000355 ) ) ;
#13729 = PRESENTATION_LAYER_ASSIGNMENT (  '', '', ( #574 ) ) ;
#13730 = DIRECTION ( 'NONE',  ( 0.000000000000000000, 0.000000000000000000, -1.000000000000000000 ) ) ;
#13731 = CARTESIAN_POINT ( 'NONE',  ( 56.65037692655918988, 61.89948385550241028, -2.184720259617163762 ) ) ;
#13732 = FACE_OUTER_BOUND ( 'NONE', #10870, .T. ) ;
#13733 = FACE_OUTER_BOUND ( 'NONE', #17318, .T. ) ;
#13734 = DIRECTION ( 'NONE',  ( 1.000000000000000000, 0.000000000000000000, 0.000000000000000000 ) ) ;
#13735 = CARTESIAN_POINT ( 'NONE',  ( 45.86712807150323812, 55.29948385550240175, -5.649768623646098220 ) ) ;
#13736 = CARTESIAN_POINT ( 'NONE',  ( 2.000000000000000000, 0.8865213383406680414, -1.535500000000000975 ) ) ;
#13737 = CARTESIAN_POINT ( 'NONE',  ( 49.97728705011486738, 59.49948385550240459, -8.000000000000001776 ) ) ;
#13738 = CIRCLE ( 'NONE', #14675, 4.799999999999999822 ) ;
#13739 = CARTESIAN_POINT ( 'NONE',  ( 42.63976443033212860, 52.00051614449766646, -0.02388180880514948964 ) ) ;
#13740 = AXIS2_PLACEMENT_3D ( 'NONE', #11131, #18618, #18811 ) ;
#13741 = CYLINDRICAL_SURFACE ( 'NONE', #17168, 4.599999999999999645 ) ;
#13742 = CYLINDRICAL_SURFACE ( 'NONE', #18195, 3.799999999999993605 ) ;
#13743 =( LENGTH_UNIT ( ) NAMED_UNIT ( * ) SI_UNIT ( .MILLI., .METRE. ) );
#13744 = MECHANICAL_DESIGN_GEOMETRIC_PRESENTATION_REPRESENTATION (  '', ( #18154 ), #8115 ) ;
#13745 = ORIENTED_EDGE ( 'NONE', *, *, #1871, .F. ) ;
#13746 = CARTESIAN_POINT ( 'NONE',  ( -74.99999999999997158, -1.000000000000000000, -5.999999999999998224 ) ) ;
#13747 = CARTESIAN_POINT ( 'NONE',  ( 45.86712807150329496, 49.70051614449766220, 5.649768623646139964 ) ) ;
#13748 = CIRCLE ( 'NONE', #17848, 3.500000000000000000 ) ;
#13749 = VECTOR ( 'NONE', #9538, 1000.000000000000000 ) ;
#13750 = CARTESIAN_POINT ( 'NONE',  ( 4.071447262713887127, -2.020725942163686284, 3.500000000000000444 ) ) ;
#13751 = DIRECTION ( 'NONE',  ( 1.000000000000000000, 0.000000000000000000, 0.000000000000000000 ) ) ;
#13752 = EDGE_LOOP ( 'NONE', ( #774, #5256, #6905, #13010, #18819 ) ) ;
#13753 = LINE ( 'NONE', #8955, #12412 ) ;
#13754 = LINE ( 'NONE', #5030, #18309 ) ;
#13755 = EDGE_CURVE ( 'NONE', #6465, #16560, #10605, .T. ) ;
#13756 = CARTESIAN_POINT ( 'NONE',  ( 44.28664221472220675, 65.09948385550239891, -1.832500667257165317 ) ) ;
#13757 = CARTESIAN_POINT ( 'NONE',  ( -2.321707774797442170, -4.824281976789052351, -0.8000000000000000444 ) ) ;
#13758 = CARTESIAN_POINT ( 'NONE',  ( 0.000000000000000000, 0.000000000000000000, -5.000000000000000000 ) ) ;
#13759 = CARTESIAN_POINT ( 'NONE',  ( 42.39856655714564226, 58.10051614449765367, -2.493737253992044156 ) ) ;
#13760 = EDGE_CURVE ( 'NONE', #15909, #16919, #10845, .T. ) ;
#13761 = CARTESIAN_POINT ( 'NONE',  ( 55.71335778527780036, 56.90051614449767214, -1.832500667257213056 ) ) ;
#13762 = DIRECTION ( 'NONE',  ( 0.000000000000000000, 0.000000000000000000, -1.000000000000000000 ) ) ;
#13763 = DIRECTION ( 'NONE',  ( 1.000000000000000000, 0.000000000000000000, 0.000000000000000000 ) ) ;
#13764 = VECTOR ( 'NONE', #12368, 1000.000000000000000 ) ;
#13765 = ORIENTED_EDGE ( 'NONE', *, *, #13168, .F. ) ;
#13766 = ORIENTED_EDGE ( 'NONE', *, *, #1846, .F. ) ;
#13767 = CARTESIAN_POINT ( 'NONE',  ( 6.207660606243411650, -2.016205878028328957, -5.000000000000000000 ) ) ;
#13768 = VERTEX_POINT ( 'NONE', #3412 ) ;
#13769 = FACE_OUTER_BOUND ( 'NONE', #16673, .T. ) ;
#13770 = AXIS2_PLACEMENT_3D ( 'NONE', #3667, #8562, #2508 ) ;
#13771 = ORIENTED_EDGE ( 'NONE', *, *, #6329, .T. ) ;
#13772 = DIRECTION ( 'NONE',  ( -1.000000000000000000, 0.000000000000000000, 0.000000000000000000 ) ) ;
#13773 = CARTESIAN_POINT ( 'NONE',  ( 56.66441430157296821, 54.09948385550240602, 2.141517661632100111 ) ) ;
#13774 = ORIENTED_EDGE ( 'NONE', *, *, #953, .T. ) ;
#13775 = CARTESIAN_POINT ( 'NONE',  ( 50.00000000000000000, 15.00000000000000000, 0.000000000000000000 ) ) ;
#13776 = ORIENTED_EDGE ( 'NONE', *, *, #11053, .T. ) ;
#13777 = CARTESIAN_POINT ( 'NONE',  ( 52.62207051974839089, 46.39948385550240317, 7.992620115222770494 ) ) ;
#13778 = AXIS2_PLACEMENT_3D ( 'NONE', #15587, #10063, #11258 ) ;
#13779 = LINE ( 'NONE', #11925, #696 ) ;
#13780 = CARTESIAN_POINT ( 'NONE',  ( 55.96859303347804371, 62.19948385550240744, 4.306917132069425946 ) ) ;
#13781 = LINE ( 'NONE', #3220, #5795 ) ;
#13782 =( NAMED_UNIT ( * ) PLANE_ANGLE_UNIT ( ) SI_UNIT ( $, .RADIAN. ) );
#13783 = VECTOR ( 'NONE', #14188, 1000.000000000000000 ) ;
#13784 = AXIS2_PLACEMENT_3D ( 'NONE', #2219, #6417, #13772 ) ;
#13785 = CARTESIAN_POINT ( 'NONE',  ( 49.97728705011495265, 55.50051614449766646, 7.000000000000000888 ) ) ;
#13786 = CARTESIAN_POINT ( 'NONE',  ( -154.9999999999999716, -14.99999999999999645, 6.499999999999999112 ) ) ;
#13787 = VECTOR ( 'NONE', #7952, 999.9999999999998863 ) ;
#13788 = CARTESIAN_POINT ( 'NONE',  ( 44.05948171654949874, 52.79948385550240175, 4.345558710429105354 ) ) ;
#13789 = FACE_OUTER_BOUND ( 'NONE', #8451, .T. ) ;
#13790 = ORIENTED_EDGE ( 'NONE', *, *, #294, .F. ) ;
#13791 = ORIENTED_EDGE ( 'NONE', *, *, #167, .T. ) ;
#13792 = DIRECTION ( 'NONE',  ( 0.000000000000000000, -1.224646799147353207E-16, 1.000000000000000000 ) ) ;
#13793 = SURFACE_SIDE_STYLE ('',( #6252 ) ) ;
#13794 = AXIS2_PLACEMENT_3D ( 'NONE', #11745, #11455, #13133 ) ;
#13795 = CARTESIAN_POINT ( 'NONE',  ( 54.13287192849676188, 54.29948385550240886, 5.649768623646098220 ) ) ;
#13796 = CARTESIAN_POINT ( 'NONE',  ( 3.973110223765528026, -0.6902454861566464928, 3.565797985667392034 ) ) ;
#13797 = CIRCLE ( 'NONE', #18835, 9.999999999999998224 ) ;
#13798 = AXIS2_PLACEMENT_3D ( 'NONE', #1123, #15735, #2315 ) ;
#13799 = EDGE_LOOP ( 'NONE', ( #448, #19384, #4474, #10490 ) ) ;
#13800 = CYLINDRICAL_SURFACE ( 'NONE', #2067, 20.00000000000000000 ) ;
#13801 =( GEOMETRIC_REPRESENTATION_CONTEXT ( 3 ) GLOBAL_UNCERTAINTY_ASSIGNED_CONTEXT ( ( #13807 ) ) GLOBAL_UNIT_ASSIGNED_CONTEXT ( ( #4325, #1386, #19353 ) ) REPRESENTATION_CONTEXT ( 'NONE', 'WORKASPACE' ) );
#13802 = ORIENTED_EDGE ( 'NONE', *, *, #11720, .T. ) ;
#13803 = CARTESIAN_POINT ( 'NONE',  ( 56.65037692655921120, 59.10051614449766078, 2.184720259617097593 ) ) ;
#13804 = EDGE_LOOP ( 'NONE', ( #5050, #11643, #19008, #7248 ) ) ;
#13805 = EDGE_CURVE ( 'NONE', #3495, #6090, #897, .T. ) ;
#13806 = CARTESIAN_POINT ( 'NONE',  ( 1.312671235360372224, 3.860931062424219462, -0.05923475698270440348 ) ) ;
#13807 = UNCERTAINTY_MEASURE_WITH_UNIT (LENGTH_MEASURE( 1.000000000000000082E-05 ), #4325, 'distance_accuracy_value', 'NONE');
#13808 = CARTESIAN_POINT ( 'NONE',  ( 0.000000000000000000, 0.000000000000000000, 0.000000000000000000 ) ) ;
#13809 = CARTESIAN_POINT ( 'NONE',  ( 44.30067958973594955, 58.10051614449765367, -1.875703265242155693 ) ) ;
#13810 = CARTESIAN_POINT ( 'NONE',  ( -19.89043790736545603, -22.09056926535314602, 9.000000000000000000 ) ) ;
#13811 = CARTESIAN_POINT ( 'NONE',  ( 44.88205777487401349, 45.80051614449766362, 3.688883143319584779 ) ) ;
#13812 = FACE_OUTER_BOUND ( 'NONE', #2774, .T. ) ;
#13813 = VECTOR ( 'NONE', #1829, 1000.000000000000000 ) ;
#13814 = CIRCLE ( 'NONE', #5365, 0.9999999999999991118 ) ;
#13815 = CARTESIAN_POINT ( 'NONE',  ( 43.20883090819742023, 62.20051614449766220, -4.963592699178938972 ) ) ;
#13816 = VERTEX_POINT ( 'NONE', #9190 ) ;
#13817 = FACE_OUTER_BOUND ( 'NONE', #5420, .T. ) ;
#13818 =( NAMED_UNIT ( * ) SI_UNIT ( $, .STERADIAN. ) SOLID_ANGLE_UNIT ( ) );
#13819 = VERTEX_POINT ( 'NONE', #7999 ) ;
#13820 = SURFACE_STYLE_USAGE ( .BOTH. , #4994 ) ;
#13821 = CONTEXT_DEPENDENT_SHAPE_REPRESENTATION ( #640, #8838 ) ;
#13822 = EDGE_CURVE ( 'NONE', #3393, #16015, #9659, .T. ) ;
#13823 = VERTEX_POINT ( 'NONE', #9472 ) ;
#13824 = CARTESIAN_POINT ( 'NONE',  ( 0.9996874511566150590, -39.97499999999999432, 0.000000000000000000 ) ) ;
#13825 = CARTESIAN_POINT ( 'NONE',  ( 3.972709601346591235, 2.746729940827189242, -2.374099244652734697 ) ) ;
#13826 = ADVANCED_FACE ( 'NONE', ( #6155 ), #12514, .T. ) ;
#13827 = CARTESIAN_POINT ( 'NONE',  ( 42.63976443033212149, 62.99948385550241170, 0.02388180880522514787 ) ) ;
#13828 = EDGE_CURVE ( 'NONE', #11277, #13101, #3230, .T. ) ;
#13829 = CARTESIAN_POINT ( 'NONE',  ( 20.00000000000000000, -20.00000000000000000, -20.00000000000000000 ) ) ;
#13830 = CARTESIAN_POINT ( 'NONE',  ( -4.078421086530219064, -3.990950201428956845, -1.000000000000000000 ) ) ;
#13831 = FACE_OUTER_BOUND ( 'NONE', #13884, .T. ) ;
#13832 = CARTESIAN_POINT ( 'NONE',  ( 55.69932041026404335, 47.89948385550240317, -1.875703265242203432 ) ) ;
#13833 = DIRECTION ( 'NONE',  ( 1.000000000000000000, 0.000000000000000000, 0.000000000000000000 ) ) ;
#13834 = CARTESIAN_POINT ( 'NONE',  ( 49.97728705011486738, 61.49948385550241170, -8.000000000000001776 ) ) ;
#13835 = CARTESIAN_POINT ( 'NONE',  ( 42.63976443033212860, 54.00051614449766646, -0.02388180880514948964 ) ) ;
#13836 = ADVANCED_FACE ( 'NONE', ( #12228 ), #7167, .T. ) ;
#13837 = EDGE_CURVE ( 'NONE', #11082, #1055, #14349, .T. ) ;
#13838 = DIRECTION ( 'NONE',  ( 1.000000000000000000, 0.000000000000000000, 0.000000000000000000 ) ) ;
#13839 = CARTESIAN_POINT ( 'NONE',  ( -74.99999999999997158, 45.00000000000001421, 15.00000000000000000 ) ) ;
#13840 = EDGE_CURVE ( 'NONE', #16268, #16243, #12470, .T. ) ;
#13841 = ORIENTED_EDGE ( 'NONE', *, *, #17298, .F. ) ;
#13842 = CARTESIAN_POINT ( 'NONE',  ( 6.452281807715818829, 2.898928808472990948, -5.021091983800339165 ) ) ;
#13843 = CARTESIAN_POINT ( 'NONE',  ( 56.65037692655921120, 45.10051614449766078, 2.184720259617097593 ) ) ;
#13844 = CARTESIAN_POINT ( 'NONE',  ( 56.65037692655918988, 63.89948385550239607, -2.184720259617163762 ) ) ;
#13845 = CIRCLE ( 'NONE', #4784, 4.799999999999999822 ) ;
#13846 = CARTESIAN_POINT ( 'NONE',  ( -17.32050807568879236, -10.00000000000004263, -9.000000000000000000 ) ) ;
#13847 = ORIENTED_EDGE ( 'NONE', *, *, #12167, .F. ) ;
#13848 = DIRECTION ( 'NONE',  ( -0.000000000000000000, -0.000000000000000000, -1.000000000000000000 ) ) ;
#13849 = CARTESIAN_POINT ( 'NONE',  ( -59.84999999999998721, 32.50000000000001421, 15.00000000000000000 ) ) ;
#13850 = CARTESIAN_POINT ( 'NONE',  ( 55.69932041026404335, 63.89948385550240317, -1.875703265242203432 ) ) ;
#13851 = LINE ( 'NONE', #18675, #1194 ) ;
#13852 =( LENGTH_UNIT ( ) NAMED_UNIT ( * ) SI_UNIT ( .MILLI., .METRE. ) );
#13853 = CARTESIAN_POINT ( 'NONE',  ( 45.31609314410960820, 58.30051614449765651, -6.485486291978072693 ) ) ;
#13854 = CARTESIAN_POINT ( 'NONE',  ( 55.11794222512599362, 56.80051614449764941, -3.688883143319583446 ) ) ;
#13855 = DIRECTION ( 'NONE',  ( 0.000000000000000000, 0.000000000000000000, -1.000000000000000000 ) ) ;
#13856 = CARTESIAN_POINT ( 'NONE',  ( -1.249999999999997558, 0.000000000000000000, 0.000000000000000000 ) ) ;
#13857 = EDGE_LOOP ( 'NONE', ( #1608, #1968, #673, #17640 ) ) ;
#13858 = ORIENTED_EDGE ( 'NONE', *, *, #9030, .T. ) ;
#13859 = CARTESIAN_POINT ( 'NONE',  ( -149.0000000000000000, -14.99999999999999645, 6.499999999999999112 ) ) ;
#13860 = ORIENTED_EDGE ( 'NONE', *, *, #7653, .F. ) ;
#13861 = ADVANCED_FACE ( 'NONE', ( #9277, #18327, #3697 ), #14367, .T. ) ;
#13862 = DIRECTION ( 'NONE',  ( 0.1836763462126260182, -0.9829867750086872524, -1.521953536530129242E-22 ) ) ;
#13863 = ORIENTED_EDGE ( 'NONE', *, *, #12157, .T. ) ;
#13864 = CARTESIAN_POINT ( 'NONE',  ( 4.211140560182196957, -2.431303136016555122, -3.745885042887436622 ) ) ;
#13865 = EDGE_CURVE ( 'NONE', #2993, #828, #951, .T. ) ;
#13866 = CARTESIAN_POINT ( 'NONE',  ( 52.29715082351547295, 52.39948385550240317, 6.992620115222774047 ) ) ;
#13867 = VERTEX_POINT ( 'NONE', #12610 ) ;
#13868 = DIRECTION ( 'NONE',  ( 0.000000000000000000, 0.000000000000000000, -1.000000000000000000 ) ) ;
#13869 = ORIENTED_EDGE ( 'NONE', *, *, #15988, .T. ) ;
#13870 = CARTESIAN_POINT ( 'NONE',  ( 56.79116909180255135, 55.79948385550239465, -4.963592699179005585 ) ) ;
#13871 = DIRECTION ( 'NONE',  ( 1.000000000000000000, 0.000000000000000000, 0.000000000000000000 ) ) ;
#13872 = CARTESIAN_POINT ( 'NONE',  ( 49.97728705011488870, 47.49948385550240459, -6.000000000000000888 ) ) ;
#13873 = CARTESIAN_POINT ( 'NONE',  ( 4.082498951862918446, 2.020725942163685396, -3.500000000000001332 ) ) ;
#13874 = CARTESIAN_POINT ( 'NONE',  ( -7.134732861516020819, -1.729090847147989773, 9.000000000000000000 ) ) ;
#13875 = CARTESIAN_POINT ( 'NONE',  ( 52.25172492374527877, 63.40051614449765793, 7.007379884777203749 ) ) ;
#13876 = DIRECTION ( 'NONE',  ( -1.000000000000000000, 0.000000000000000000, 0.000000000000000000 ) ) ;
#13877 = CARTESIAN_POINT ( 'NONE',  ( 55.96859303347804371, 58.19948385550241454, 4.306917132069425946 ) ) ;
#13878 = CARTESIAN_POINT ( 'NONE',  ( 2.449293598294706513E-15, -20.00000000000000000, -9.000000000000000000 ) ) ;
#13879 = ORIENTED_EDGE ( 'NONE', *, *, #18537, .F. ) ;
#13880 = DIRECTION ( 'NONE',  ( 1.000000000000000000, 0.000000000000000000, 0.000000000000000000 ) ) ;
#13881 = AXIS2_PLACEMENT_3D ( 'NONE', #17322, #3879, #10227 ) ;
#13882 = CARTESIAN_POINT ( 'NONE',  ( 45.86712807150323812, 51.29948385550240175, -5.649768623646098220 ) ) ;
#13883 = SURFACE_SIDE_STYLE ('',( #6439 ) ) ;
#13884 = EDGE_LOOP ( 'NONE', ( #4280, #15461, #1955, #4649 ) ) ;
#13885 = AXIS2_PLACEMENT_3D ( 'NONE', #18486, #17103, #3757 ) ;
#13886 = CARTESIAN_POINT ( 'NONE',  ( 1.250000000000001110, 0.000000000000000000, 0.000000000000000000 ) ) ;
#13887 = B_SPLINE_CURVE_WITH_KNOTS ( 'NONE', 3,
 ( #3185, #9145, #3268, #509 ),
 .UNSPECIFIED., .F., .F.,
 ( 4, 4 ),
 ( 0.000000000000000000, 0.002452478801916361129 ),
 .UNSPECIFIED. ) ;
#13888 = ORIENTED_EDGE ( 'NONE', *, *, #1800, .F. ) ;
#13889 = DIRECTION ( 'NONE',  ( 1.000000000000000000, -0.000000000000000000, 0.000000000000000000 ) ) ;
#13890 = VERTEX_POINT ( 'NONE', #3988 ) ;
#13891 = DIRECTION ( 'NONE',  ( 0.000000000000000000, 0.000000000000000000, -1.000000000000000000 ) ) ;
#13892 = DIRECTION ( 'NONE',  ( 0.000000000000000000, 0.000000000000000000, -1.000000000000000000 ) ) ;
#13893 = CARTESIAN_POINT ( 'NONE',  ( 55.69932041026405045, 61.10051614449766788, 1.875703265242156359 ) ) ;
#13894 = PLANE ( 'NONE',  #4847 ) ;
#13895 = AXIS2_PLACEMENT_3D ( 'NONE', #5316, #13157, #7177 ) ;
#13896 = CARTESIAN_POINT ( 'NONE',  ( -74.99999999999997158, 32.50000000000001421, -9.999999999999998224 ) ) ;
#13897 = CARTESIAN_POINT ( 'NONE',  ( 0.000000000000000000, 0.000000000000000000, -4.000000000000000000 ) ) ;
#13898 = VECTOR ( 'NONE', #11073, 1000.000000000000000 ) ;
#13899 = CARTESIAN_POINT ( 'NONE',  ( 52.57664461997821093, 59.40051614449765793, 8.007379884777206414 ) ) ;
#13900 = EDGE_LOOP ( 'NONE', ( #18381, #15247 ) ) ;
#13901 = ORIENTED_EDGE ( 'NONE', *, *, #14789, .F. ) ;
#13902 = CARTESIAN_POINT ( 'NONE',  ( -154.9999999999999716, -14.99999999999999645, 17.00000000000000000 ) ) ;
#13903 =( NAMED_UNIT ( * ) SI_UNIT ( $, .STERADIAN. ) SOLID_ANGLE_UNIT ( ) );
#13904 = ORIENTED_EDGE ( 'NONE', *, *, #2195, .T. ) ;
#13905 = CONTEXT_DEPENDENT_SHAPE_REPRESENTATION ( #15411, #5379 ) ;
#13906 = ORIENTED_EDGE ( 'NONE', *, *, #1782, .T. ) ;
#13907 = DIRECTION ( 'NONE',  ( 9.710251638871371392E-17, 5.969973981896233748E-17, 1.000000000000000000 ) ) ;
#13908 = CARTESIAN_POINT ( 'NONE',  ( -2.500000000000000444, 3.061616997868383634E-16, -5.000000000000000888 ) ) ;
#13909 = AXIS2_PLACEMENT_3D ( 'NONE', #2950, #17661, #7258 ) ;
#13910 = LINE ( 'NONE', #9592, #9709 ) ;
#13911 = CARTESIAN_POINT ( 'NONE',  ( -62.49999999999997158, 20.00000000000001421, -15.00000000000000000 ) ) ;
#13912 = CARTESIAN_POINT ( 'NONE',  ( -72.99999999999997158, 2.999999999999999112, 5.999999999999998224 ) ) ;
#13913 = CARTESIAN_POINT ( 'NONE',  ( 14.86289650954772590, -6.617387872822656725, -9.000000000000000000 ) ) ;
#13914 = CARTESIAN_POINT ( 'NONE',  ( 52.29715082351547295, 62.39948385550239607, 6.992620115222774047 ) ) ;
#13915 = CARTESIAN_POINT ( 'NONE',  ( 6.534838248920899595, 5.903531555104835071, 8.098083288904839678E-18 ) ) ;
#13916 = CARTESIAN_POINT ( 'NONE',  ( 41.58830220609386430, 62.99948385550241170, 0.02388180880523263147 ) ) ;
#13917 = CARTESIAN_POINT ( 'NONE',  ( 54.09612160359792199, 61.30051614449766362, 5.676469297603124353 ) ) ;
#13918 = AXIS2_PLACEMENT_3D ( 'NONE', #17369, #4688, #3124 ) ;
#13919 = SHAPE_REPRESENTATION ( 'circlip for shafts normal_din_Circlip DIN 471 - 8 x 0.8', ( #10359 ), #12491 ) ;
#13920 = DIRECTION ( 'NONE',  ( 0.000000000000000000, 0.000000000000000000, 1.000000000000000000 ) ) ;
#13921 = CARTESIAN_POINT ( 'NONE',  ( 4.071447262713887127, -2.020725942163686284, 3.500000000000000444 ) ) ;
#13922 = EDGE_CURVE ( 'NONE', #18142, #16469, #15759, .T. ) ;
#13923 = SURFACE_STYLE_FILL_AREA ( #16797 ) ;
#13924 = ORIENTED_EDGE ( 'NONE', *, *, #14802, .T. ) ;
#13925 = AXIS2_PLACEMENT_3D ( 'NONE', #11066, #5184, #11257 ) ;
#13926 = ADVANCED_FACE ( 'NONE', ( #2244 ), #1859, .F. ) ;
#13927 = PLANE ( 'NONE',  #1567 ) ;
#13928 = CARTESIAN_POINT ( 'NONE',  ( 50.02271294988505446, 48.50051614449765935, -7.000000000000000888 ) ) ;
#13929 = EDGE_CURVE ( 'NONE', #6422, #8729, #19087, .T. ) ;
#13930 = EDGE_CURVE ( 'NONE', #2647, #2843, #19408, .T. ) ;
#13931 = CARTESIAN_POINT ( 'NONE',  ( 57.36023556966787851, 61.99948385550241170, -0.02388180880522424582 ) ) ;
#13932 = CARTESIAN_POINT ( 'NONE',  ( -4.158233816355195955, -0.4370479853238878887, -9.000000000000000000 ) ) ;
#13933 = VERTEX_POINT ( 'NONE', #2435 ) ;
#13934 = CYLINDRICAL_SURFACE ( 'NONE', #10204, 8.000000000000007105 ) ;
#13935 = LINE ( 'NONE', #8054, #4831 ) ;
#13936 = CARTESIAN_POINT ( 'NONE',  ( 53.54508667620428497, 62.29948385550241596, 4.840751629271157874 ) ) ;
#13937 = CARTESIAN_POINT ( 'NONE',  ( 2.595115354961440524, -7.673029147243177306, -1.000000000000000000 ) ) ;
#13938 = CARTESIAN_POINT ( 'NONE',  ( 47.70284917648453415, 47.39948385550238896, -6.992620115222774047 ) ) ;
#13939 = LINE ( 'NONE', #3565, #9810 ) ;
#13940 = CARTESIAN_POINT ( 'NONE',  ( 45.27934281921082516, 59.70051614449766220, 6.458785618021089192 ) ) ;
#13941 = AXIS2_PLACEMENT_3D ( 'NONE', #7441, #7537, #1756 ) ;
#13942 = CARTESIAN_POINT ( 'NONE',  ( 57.36023556966787851, 45.00051614449763804, 0.02388180880515038476 ) ) ;
#13943 = DIRECTION ( 'NONE',  ( 1.000000000000000000, 0.000000000000000000, 0.000000000000000000 ) ) ;
#13944 = CARTESIAN_POINT ( 'NONE',  ( 6.204460410672267834, -4.828986228461502606, -1.635950503254466337 ) ) ;
#13946 = EDGE_LOOP ( 'NONE', ( #187, #12884, #14615, #2516 ) ) ;
#13945 = EDGE_CURVE ( 'NONE', #11405, #3727, #1051, .T. ) ;
#13947 = AXIS2_PLACEMENT_3D ( 'NONE', #16365, #14774, #9087 ) ;
#13948 = ADVANCED_FACE ( 'NONE', ( #15658 ), #588, .T. ) ;
#13949 = EDGE_LOOP ( 'NONE', ( #10056, #11709, #5279, #12639 ) ) ;
#13950 = CARTESIAN_POINT ( 'NONE',  ( 6.541171952014627422, 2.986180817377861896, -5.112746308113085725 ) ) ;
#13951 = ORIENTED_EDGE ( 'NONE', *, *, #6503, .T. ) ;
#13952 = CARTESIAN_POINT ( 'NONE',  ( 0.8816464618332836567, -24.71833652004169934, 9.999999999999998224 ) ) ;
#13953 = ORIENTED_EDGE ( 'NONE', *, *, #6378, .T. ) ;
#13954 = DIRECTION ( 'NONE',  ( -0.9995917534020515305, -0.02857142857142857054, 0.000000000000000000 ) ) ;
#13955 = CARTESIAN_POINT ( 'NONE',  ( 55.96859303347805081, 50.19948385550240744, 4.306917132069425058 ) ) ;
#13956 = VERTEX_POINT ( 'NONE', #14472 ) ;
#13957 = DIRECTION ( 'NONE',  ( 1.000000000000000000, 0.000000000000000000, 0.000000000000000000 ) ) ;
#13958 = ORIENTED_EDGE ( 'NONE', *, *, #18157, .T. ) ;
#13959 = CARTESIAN_POINT ( 'NONE',  ( 54.68390685589033495, 55.69948385550240744, -6.485486291978119766 ) ) ;
#13960 = CARTESIAN_POINT ( 'NONE',  ( 50.00000000000000000, 15.00000000000000000, 4.000000000000003553 ) ) ;
#13961 = CARTESIAN_POINT ( 'NONE',  ( 50.02271294988511841, 46.49948385550240459, 6.000000000000000888 ) ) ;
#13962 = FACE_OUTER_BOUND ( 'NONE', #3864, .T. ) ;
#13963 = CARTESIAN_POINT ( 'NONE',  ( 4.132952817037861770, -4.063368025374527015, 6.968404583626299416E-17 ) ) ;
#13964 = CARTESIAN_POINT ( 'NONE',  ( 42.63976443033212860, 60.00051614449764514, -0.02388180880514948964 ) ) ;
#13965 = DIRECTION ( 'NONE',  ( 0.000000000000000000, 0.000000000000000000, -1.000000000000000000 ) ) ;
#13966 = CARTESIAN_POINT ( 'NONE',  ( 43.33558569842703179, 61.09948385550240602, -2.141517661632099223 ) ) ;
#13967 = CARTESIAN_POINT ( 'NONE',  ( 9.037824375505316254, -2.158539001597377105, 9.000000000000000000 ) ) ;
#13968 = VECTOR ( 'NONE', #4755, 1000.000000000000000 ) ;
#13969 = ORIENTED_EDGE ( 'NONE', *, *, #7471, .F. ) ;
#13970 = ADVANCED_FACE ( 'NONE', ( #2335 ), #6230, .T. ) ;
#13971 = ORIENTED_EDGE ( 'NONE', *, *, #11349, .T. ) ;
#13972 = CARTESIAN_POINT ( 'NONE',  ( -154.9999999999999716, -14.99999999999999645, -4.000000000000000000 ) ) ;
#13973 = ADVANCED_FACE ( 'NONE', ( #850 ), #9966, .F. ) ;
#13974 = CARTESIAN_POINT ( 'NONE',  ( 47.70284917648453415, 51.39948385550238896, -6.992620115222774047 ) ) ;
#13975 = ORIENTED_EDGE ( 'NONE', *, *, #15500, .F. ) ;
#13976 = ORIENTED_EDGE ( 'NONE', *, *, #17812, .T. ) ;
#13977 = CARTESIAN_POINT ( 'NONE',  ( -158.9999999999999716, -14.99999999999999645, 10.00000000000000000 ) ) ;
#13978 = AXIS2_PLACEMENT_3D ( 'NONE', #5343, #12795, #6806 ) ;
#13979 = EDGE_LOOP ( 'NONE', ( #15177, #10668, #630, #9956 ) ) ;
#13980 = DIRECTION ( 'NONE',  ( 0.000000000000000000, 0.000000000000000000, -1.000000000000000000 ) ) ;
#13981 = ORIENTED_EDGE ( 'NONE', *, *, #16972, .F. ) ;
#13982 = AXIS2_PLACEMENT_3D ( 'NONE', #1958, #3519, #9483 ) ;
#13983 = CARTESIAN_POINT ( 'NONE',  ( 52.29715082351547295, 46.39948385550240317, 6.992620115222774047 ) ) ;
#13984 = PRODUCT_DEFINITION_CONTEXT ( 'detailed design', #13412, 'design' ) ;
#13985 = CARTESIAN_POINT ( 'NONE',  ( 3.999999999999999112, 1.941961291383486277, -0.3515519931180248192 ) ) ;
#13986 = CARTESIAN_POINT ( 'NONE',  ( 43.69122665457040000, 64.00051614449765225, -0.02388180880515696977 ) ) ;
#13987 = LINE ( 'NONE', #6548, #464 ) ;
#13988 = EDGE_CURVE ( 'NONE', #6680, #12254, #9037, .T. ) ;
#13989 = DIRECTION ( 'NONE',  ( 1.000000000000000000, 0.000000000000000000, 0.000000000000000000 ) ) ;
#13990 = CARTESIAN_POINT ( 'NONE',  ( -16.32050807568872841, -30.00000000000008171, -9.000000000000000000 ) ) ;
#13991 = CIRCLE ( 'NONE', #8372, 2.000000000000000888 ) ;
#13992 = CARTESIAN_POINT ( 'NONE',  ( 52.62207051974829852, 60.60051614449765367, -7.992620115222797139 ) ) ;
#13993 = ADVANCED_FACE ( 'NONE', ( #7018 ), #5359, .T. ) ;
#13994 = CIRCLE ( 'NONE', #5553, 0.9999999999999985567 ) ;
#13995 = ORIENTED_EDGE ( 'NONE', *, *, #2601, .F. ) ;
#13996 = EDGE_LOOP ( 'NONE', ( #5328, #18030, #13709, #14884 ) ) ;
#13997 = CARTESIAN_POINT ( 'NONE',  ( -14.14213562373094213, -14.99999999999998757, -23.00000000000000000 ) ) ;
#13998 = COLOUR_RGB ( '',0.8941176470588234615, 0.8941176470588234615, 0.8941176470588234615 ) ;
#13999 = LINE ( 'NONE', #12346, #14379 ) ;
#14000 = APPLICATION_PROTOCOL_DEFINITION ( 'draft international standard', 'automotive_design', 1998, #11024 ) ;
#14001 = ORIENTED_EDGE ( 'NONE', *, *, #14553, .F. ) ;
#14002 = DIRECTION ( 'NONE',  ( -0.000000000000000000, 0.000000000000000000, 1.000000000000000000 ) ) ;
#14003 = DIRECTION ( 'NONE',  ( 1.000000000000000000, 0.000000000000000000, 0.000000000000000000 ) ) ;
#14004 = ORIENTED_EDGE ( 'NONE', *, *, #1375, .T. ) ;
#14005 = VECTOR ( 'NONE', #814, 1000.000000000000000 ) ;
#14006 = CONICAL_SURFACE ( 'NONE', #11506, 8.105212085995399107, 1.221730476396037490 ) ;
#14007 = DIRECTION ( 'NONE',  ( 0.000000000000000000, 0.000000000000000000, 1.000000000000000000 ) ) ;
#14008 = CARTESIAN_POINT ( 'NONE',  ( 4.071447262713887127, 2.020725942163688504, 3.500000000000000000 ) ) ;
#14009 = DIRECTION ( 'NONE',  ( 0.000000000000000000, -1.000000000000000000, 8.673617379884035472E-16 ) ) ;
#14010 = CARTESIAN_POINT ( 'NONE',  ( 62.49999999999998579, 0.000000000000000000, -9.999999999999998224 ) ) ;
#14011 = CARTESIAN_POINT ( 'NONE',  ( 49.97728705011488870, 45.49948385550240459, -6.000000000000000888 ) ) ;
#14012 = STYLED_ITEM ( 'NONE', ( #4623 ), #8491 ) ;
#14013 = CARTESIAN_POINT ( 'NONE',  ( 2.141980652367355464, -6.189445006155633422, 0.000000000000000000 ) ) ;
#14014 = CARTESIAN_POINT ( 'NONE',  ( 57.61547081786812896, 58.09948385550241312, 2.450534656007040901 ) ) ;
#14015 = CARTESIAN_POINT ( 'NONE',  ( 44.03140696652198471, 61.80051614449767072, 4.306917132069485454 ) ) ;
#14016 = CARTESIAN_POINT ( 'NONE',  ( 5.100000000000002309, 0.000000000000000000, 0.000000000000000000 ) ) ;
#14017 = DIRECTION ( 'NONE',  ( 1.000000000000000000, 0.000000000000000000, 0.000000000000000000 ) ) ;
#14018 = CIRCLE ( 'NONE', #10275, 2.649999999999985700 ) ;
#14019 = VECTOR ( 'NONE', #13218, 1000.000000000000000 ) ;
#14020 = PRODUCT_CONTEXT ( 'NONE', #8769, 'mechanical' ) ;
#14021 =( REPRESENTATION_RELATIONSHIP ('NONE','NONE', #16703, #13919 ) REPRESENTATION_RELATIONSHIP_WITH_TRANSFORMATION ( #875 )SHAPE_REPRESENTATION_RELATIONSHIP( ) );
#14022 = EDGE_LOOP ( 'NONE', ( #5726, #13273, #15852, #17451 ) ) ;
#14023 = CARTESIAN_POINT ( 'NONE',  ( -179.9999999999999716, -15.00000000000000000, -3.999999999999999112 ) ) ;
#14024 = CARTESIAN_POINT ( 'NONE',  ( 54.09612160359792199, 47.30051614449765651, 5.676469297603124353 ) ) ;
#14025 = DIRECTION ( 'NONE',  ( -0.000000000000000000, -0.000000000000000000, -1.000000000000000000 ) ) ;
#14026 = DIRECTION ( 'NONE',  ( -0.000000000000000000, 0.000000000000000000, 1.000000000000000000 ) ) ;
#14027 = VERTEX_POINT ( 'NONE', #661 ) ;
#14028 = CARTESIAN_POINT ( 'NONE',  ( 5.599999999999998757, 0.000000000000000000, 5.200000000000001066 ) ) ;
#14029 = DIRECTION ( 'NONE',  ( 1.000000000000000000, 0.000000000000000000, 0.000000000000000000 ) ) ;
#14030 = EDGE_CURVE ( 'NONE', #14839, #3297, #3317, .T. ) ;
#14031 = AXIS2_PLACEMENT_3D ( 'NONE', #379, #7717, #10753 ) ;
#14032 = CARTESIAN_POINT ( 'NONE',  ( 51.97223112728254790, 64.39948385550239607, 5.992620115222778487 ) ) ;
#14033 = DIRECTION ( 'NONE',  ( -0.000000000000000000, -0.000000000000000000, 1.000000000000000000 ) ) ;
#14034 = DIRECTION ( 'NONE',  ( -0.000000000000000000, -0.000000000000000000, 1.000000000000000000 ) ) ;
#14035 = B_SPLINE_CURVE_WITH_KNOTS ( 'NONE', 3,
 ( #8470, #14343, #15929, #1032 ),
 .UNSPECIFIED., .F., .F.,
 ( 4, 4 ),
 ( 0.002977824986803813152, 0.005972417098209346735 ),
 .UNSPECIFIED. ) ;
#14036 = CARTESIAN_POINT ( 'NONE',  ( 52.57664461997821093, 59.40051614449765793, 8.007379884777206414 ) ) ;
#14037 = CARTESIAN_POINT ( 'NONE',  ( 55.71335778527780036, 58.90051614449766504, -1.832500667257213056 ) ) ;
#14038 = COLOUR_RGB ( '',1.000000000000000000, 0.9490196078431372140, 0.9098039215686274384 ) ;
#14039 = FACE_OUTER_BOUND ( 'NONE', #9383, .T. ) ;
#14040 = DIRECTION ( 'NONE',  ( 1.000000000000000000, 0.000000000000000000, 0.000000000000000000 ) ) ;
#14041 = ORIENTED_EDGE ( 'NONE', *, *, #1734, .T. ) ;
#14042 = ADVANCED_FACE ( 'NONE', ( #8097, #5257, #2134 ), #14074, .T. ) ;
#14043 = EDGE_CURVE ( 'NONE', #11186, #17731, #12792, .T. ) ;
#14044 = ORIENTED_EDGE ( 'NONE', *, *, #11956, .T. ) ;
#14045 = DIRECTION ( 'NONE',  ( 0.000000000000000000, 0.000000000000000000, 1.000000000000000000 ) ) ;
#14046 = EDGE_LOOP ( 'NONE', ( #15604, #18604, #15373 ) ) ;
#14047 = AXIS2_PLACEMENT_3D ( 'NONE', #15239, #1820, #18399 ) ;
#14048 = EDGE_CURVE ( 'NONE', #5656, #17997, #14169, .T. ) ;
#14049 = DIRECTION ( 'NONE',  ( 1.000000000000000000, 0.000000000000000000, -0.000000000000000000 ) ) ;
#14050 = EDGE_CURVE ( 'NONE', #18826, #62, #6839, .T. ) ;
#14051 = ORIENTED_EDGE ( 'NONE', *, *, #6565, .T. ) ;
#14052 = CARTESIAN_POINT ( 'NONE',  ( -2.100000000000000089, 2.571758278209441957E-16, -5.000000000000000000 ) ) ;
#14053 = CARTESIAN_POINT ( 'NONE',  ( 56.65037692655918988, 49.89948385550240317, -2.184720259617163762 ) ) ;
#14054 = VERTEX_POINT ( 'NONE', #7215 ) ;
#14055 = STYLED_ITEM ( 'NONE', ( #1895 ), #6604 ) ;
#14056 = CARTESIAN_POINT ( 'NONE',  ( 6.481779955677435368, -2.910222513313295511, -5.040653254389411586 ) ) ;
#14057 = ORIENTED_EDGE ( 'NONE', *, *, #10604, .T. ) ;
#14058 = CARTESIAN_POINT ( 'NONE',  ( 49.97728705011486738, 51.49948385550240459, -8.000000000000001776 ) ) ;
#14059 = CARTESIAN_POINT ( 'NONE',  ( -7.134732861515892033, -38.27090915285207018, -9.000000000000000000 ) ) ;
#14060 = ADVANCED_FACE ( 'NONE', ( #13094 ), #2818, .F. ) ;
#14061 = CARTESIAN_POINT ( 'NONE',  ( 49.97728705011488870, 45.49948385550240459, -6.000000000000000888 ) ) ;
#14062 = DIRECTION ( 'NONE',  ( 0.000000000000000000, -1.000000000000000000, 0.000000000000000000 ) ) ;
#14063 = ADVANCED_FACE ( 'NONE', ( #1144 ), #1435, .T. ) ;
#14064 = CARTESIAN_POINT ( 'NONE',  ( -0.5000000000000000000, -6.429618962271402616, -1.000000000000000000 ) ) ;
#14065 = CARTESIAN_POINT ( 'NONE',  ( 44.03140696652198471, 57.80051614449766362, 4.306917132069485454 ) ) ;
#14066 = AXIS2_PLACEMENT_3D ( 'NONE', #7654, #211, #18361 ) ;
#14067 = CARTESIAN_POINT ( 'NONE',  ( 43.33558569842703179, 57.09948385550240602, -2.141517661632099223 ) ) ;
#14068 = CARTESIAN_POINT ( 'NONE',  ( 6.533910050139697390, -5.901028503456124064, 1.992084869049455159E-14 ) ) ;
#14069 = DIRECTION ( 'NONE',  ( -0.9768494444668812671, -0.2139279384389642935, 0.000000000000000000 ) ) ;
#14070 = ORIENTED_EDGE ( 'NONE', *, *, #10100, .T. ) ;
#14071 = EDGE_CURVE ( 'NONE', #10468, #8619, #3111, .T. ) ;
#14072 = CIRCLE ( 'NONE', #5629, 2.649999999999989697 ) ;
#14073 = ORIENTED_EDGE ( 'NONE', *, *, #5127, .T. ) ;
#14074 = PLANE ( 'NONE',  #4673 ) ;
#14075 = SHAPE_REPRESENTATION_RELATIONSHIP ( 'NONE' , 'NONE' ,  #17450, #11045 ) ;
#14076 = CARTESIAN_POINT ( 'NONE',  ( 56.66441430157296821, 50.09948385550240602, 2.141517661632100111 ) ) ;
#14077 = EDGE_LOOP ( 'NONE', ( #15225, #12785, #7421, #13858, #11018, #12585 ) ) ;
#14078 = ORIENTED_EDGE ( 'NONE', *, *, #4507, .F. ) ;
#14079 = DIRECTION ( 'NONE',  ( -1.000000000000000000, 0.000000000000000000, 0.000000000000000000 ) ) ;
#14080 = VECTOR ( 'NONE', #11971, 1000.000000000000000 ) ;
#14081 = ORIENTED_EDGE ( 'NONE', *, *, #344, .T. ) ;
#14082 = VECTOR ( 'NONE', #9319, 1000.000000000000000 ) ;
#14083 = CARTESIAN_POINT ( 'NONE',  ( 44.05948171654945611, 64.20051614449766930, -4.345558710429044069 ) ) ;
#14084 = AXIS2_PLACEMENT_3D ( 'NONE', #6706, #5048, #12304 ) ;
#14085 = ORIENTED_EDGE ( 'NONE', *, *, #14954, .F. ) ;
#14086 = CARTESIAN_POINT ( 'NONE',  ( 0.000000000000000000, 0.000000000000000000, 10.00000000000000000 ) ) ;
#14087 = CIRCLE ( 'NONE', #5012, 0.1000000000000011297 ) ;
#14088 = CARTESIAN_POINT ( 'NONE',  ( 53.54508667620424234, 60.70051614449766930, -4.840751629271188961 ) ) ;
#14089 = CARTESIAN_POINT ( 'NONE',  ( 17.32050807568887052, -29.99999999999984013, -9.000000000000000000 ) ) ;
#14090 = DIRECTION ( 'NONE',  ( 0.000000000000000000, 0.000000000000000000, 1.000000000000000000 ) ) ;
#14091 = VECTOR ( 'NONE', #10179, 1000.000000000000000 ) ;
#14092 = CARTESIAN_POINT ( 'NONE',  ( 45.27934281921082516, 61.70051614449766220, 6.458785618021089192 ) ) ;
#14093 = VECTOR ( 'NONE', #6652, 1000.000000000000000 ) ;
#14094 = VECTOR ( 'NONE', #18892, 1000.000000000000000 ) ;
#14095 = ORIENTED_EDGE ( 'NONE', *, *, #13531, .T. ) ;
#14096 = ORIENTED_EDGE ( 'NONE', *, *, #893, .F. ) ;
#14097 = DIRECTION ( 'NONE',  ( 0.000000000000000000, 0.000000000000000000, -1.000000000000000000 ) ) ;
#14098 = DIRECTION ( 'NONE',  ( 0.000000000000000000, 0.000000000000000000, 1.000000000000000000 ) ) ;
#14099 = ITEM_DEFINED_TRANSFORMATION ( 'NONE', 'NONE', #11672,  #10359 ) ;
#14100 = VECTOR ( 'NONE', #1894, 1000.000000000000000 ) ;
#14101 = VERTEX_POINT ( 'NONE', #11911 ) ;
#14102 = CARTESIAN_POINT ( 'NONE',  ( 6.244297270355322560, -0.4917101305082151597, -5.105276777067913052 ) ) ;
#14103 = EDGE_CURVE ( 'NONE', #6513, #2794, #5946, .T. ) ;
#14104 = CARTESIAN_POINT ( 'NONE',  ( 10.00000000000000000, 15.00000000000001776, 15.00000000000000000 ) ) ;
#14105 = ORIENTED_EDGE ( 'NONE', *, *, #18888, .F. ) ;
#14106 = CIRCLE ( 'NONE', #11607, 4.000000000000003553 ) ;
#14107 = EDGE_CURVE ( 'NONE', #5700, #8510, #3008, .T. ) ;
#14108 = DIRECTION ( 'NONE',  ( 0.000000000000000000, 0.000000000000000000, 1.000000000000000000 ) ) ;
#14109 = CARTESIAN_POINT ( 'NONE',  ( 0.4465819873851989974, -2.886751345948120218, 4.999999999999999112 ) ) ;
#14110 = CARTESIAN_POINT ( 'NONE',  ( 0.000000000000000000, 0.000000000000000000, 0.000000000000000000 ) ) ;
#14111 = AXIS2_PLACEMENT_3D ( 'NONE', #17929, #1444, #14865 ) ;
#14112 = CARTESIAN_POINT ( 'NONE',  ( 10.00000000000000000, 25.00000000000001776, 15.00000000000000000 ) ) ;
#14113 = CARTESIAN_POINT ( 'NONE',  ( 25.00000000000000711, -20.00000000000000000, -23.00000000000000000 ) ) ;
#14114 = CARTESIAN_POINT ( 'NONE',  ( 44.05948171654949874, 62.79948385550241596, 4.345558710429105354 ) ) ;
#14115 = DIRECTION ( 'NONE',  ( -0.000000000000000000, -0.000000000000000000, -1.000000000000000000 ) ) ;
#14116 = CARTESIAN_POINT ( 'NONE',  ( 57.61547081786812896, 60.09948385550240602, 2.450534656007040901 ) ) ;
#14117 = CARTESIAN_POINT ( 'NONE',  ( 47.70284917648459100, 63.60051614449766078, 6.992620115222796251 ) ) ;
#14118 = CARTESIAN_POINT ( 'NONE',  ( -20.63749999999999574, 7.347880794884121708E-16, 6.000000000000001776 ) ) ;
#14119 = DIRECTION ( 'NONE',  ( 1.000000000000000000, 0.000000000000000000, 0.000000000000000000 ) ) ;
#14120 = CIRCLE ( 'NONE', #10690, 4.000000000000003553 ) ;
#14121 = EDGE_LOOP ( 'NONE', ( #10313, #5517, #6248, #13049 ) ) ;
#14122 = CIRCLE ( 'NONE', #990, 4.000000000000003553 ) ;
#14123 =( LENGTH_UNIT ( ) NAMED_UNIT ( * ) SI_UNIT ( .MILLI., .METRE. ) );
#14124 = PRODUCT_DEFINITION_SHAPE ( 'NONE', 'NONE',  #10570 ) ;
#14125 = COLOUR_RGB ( '',0.8941176470588234615, 0.8941176470588234615, 0.8941176470588234615 ) ;
#14126 = DIRECTION ( 'NONE',  ( 0.000000000000000000, 0.000000000000000000, -1.000000000000000000 ) ) ;
#14127 = CARTESIAN_POINT ( 'NONE',  ( 55.94051828345054389, 51.20051614449765509, 4.345558710429044957 ) ) ;
#14128 = LINE ( 'NONE', #17387, #4998 ) ;
#14129 = DIRECTION ( 'NONE',  ( 1.000000000000000000, -1.734723475976807341E-16, -0.000000000000000000 ) ) ;
#14130 = ORIENTED_EDGE ( 'NONE', *, *, #13241, .T. ) ;
#14131 = CARTESIAN_POINT ( 'NONE',  ( 2.449293598294706513E-15, -20.00000000000000000, 15.00000000000000355 ) ) ;
#14132 = DIRECTION ( 'NONE',  ( 0.000000000000000000, 0.000000000000000000, -1.000000000000000000 ) ) ;
#14133 = DIRECTION ( 'NONE',  ( -4.082155997157844188E-16, 1.000000000000000000, 0.000000000000000000 ) ) ;
#14134 = CARTESIAN_POINT ( 'NONE',  ( 45.90387839640214196, 46.69948385550240744, 5.676469297603166098 ) ) ;
#14135 = CARTESIAN_POINT ( 'NONE',  ( -0.5000000000000000000, -6.429618962271402616, 0.000000000000000000 ) ) ;
#14136 = CARTESIAN_POINT ( 'NONE',  ( 56.81924384183006538, 60.80051614449766362, -4.924951120819380357 ) ) ;
#14137 = CARTESIAN_POINT ( 'NONE',  ( 50.02271294988506156, 60.50051614449766646, -6.000000000000000888 ) ) ;
#14138 = CIRCLE ( 'NONE', #10076, 24.99999999999999289 ) ;
#14139 = DIRECTION ( 'NONE',  ( 1.000000000000000000, 0.000000000000000000, 0.000000000000000000 ) ) ;
#14140 = CARTESIAN_POINT ( 'NONE',  ( 4.000000000000003553, 4.286263797015736595E-16, -3.500000000000000000 ) ) ;
#14141 = VERTEX_POINT ( 'NONE', #17917 ) ;
#14142 = EDGE_LOOP ( 'NONE', ( #975, #2632, #7775, #2912 ) ) ;
#14143 = ORIENTED_EDGE ( 'NONE', *, *, #4680, .T. ) ;
#14144 = CARTESIAN_POINT ( 'NONE',  ( -154.9999999999999716, -14.99999999999999645, -17.00000000000000000 ) ) ;
#14145 = ORIENTED_EDGE ( 'NONE', *, *, #17545, .F. ) ;
#14146 = ADVANCED_FACE ( 'NONE', ( #7506 ), #8095, .T. ) ;
#14147 = LINE ( 'NONE', #731, #6244 ) ;
#14148 = CIRCLE ( 'NONE', #1971, 1.000000000000000222 ) ;
#14149 = EDGE_LOOP ( 'NONE', ( #5895, #16347, #11399, #14490 ) ) ;
#14150 = CARTESIAN_POINT ( 'NONE',  ( -20.00000000000000000, -19.99999999999999289, -20.00000000000000000 ) ) ;
#14151 = CARTESIAN_POINT ( 'NONE',  ( 44.05948171654949874, 60.79948385550240886, 4.345558710429104465 ) ) ;
#14152 = ORIENTED_EDGE ( 'NONE', *, *, #14162, .T. ) ;
#14153 = CARTESIAN_POINT ( 'NONE',  ( -0.6507732100473471171, 4.243078065514775510, -0.2236248678334823436 ) ) ;
#14154 = ORIENTED_EDGE ( 'NONE', *, *, #1987, .F. ) ;
#14155 = CARTESIAN_POINT ( 'NONE',  ( 50.02271294988513972, 54.49948385550240459, 8.000000000000001776 ) ) ;
#14156 = CARTESIAN_POINT ( 'NONE',  ( -158.7998746980210001, -15.03085902363206472, 15.79999999999999893 ) ) ;
#14157 = CARTESIAN_POINT ( 'NONE',  ( 54.09612160359786515, 63.69948385550240744, -5.676469297603166098 ) ) ;
#14158 = CARTESIAN_POINT ( 'NONE',  ( 3.972066048304770725, 3.435565134476467275, 1.180968096049824556 ) ) ;
#14159 = PLANE ( 'NONE',  #5876 ) ;
#14160 = CARTESIAN_POINT ( 'NONE',  ( 57.36023556966787851, 61.00051614449766646, 0.02388180880515038476 ) ) ;
#14161 = CARTESIAN_POINT ( 'NONE',  ( 43.69122665457040000, 46.00051614449764514, -0.02388180880515696977 ) ) ;
#14162 = EDGE_CURVE ( 'NONE', #2538, #3923, #5298, .T. ) ;
#14163 = CARTESIAN_POINT ( 'NONE',  ( 45.90387839640214196, 58.69948385550240033, 5.676469297603166098 ) ) ;
#14164 = DIRECTION ( 'NONE',  ( -0.000000000000000000, -0.000000000000000000, 1.000000000000000000 ) ) ;
#14165 = CARTESIAN_POINT ( 'NONE',  ( -5.384454397937118664, 6.594054843588581554E-16, -4.484454397937119197 ) ) ;
#14166 = ORIENTED_EDGE ( 'NONE', *, *, #10811, .T. ) ;
#14167 = PRODUCT_DEFINITION_FORMATION_WITH_SPECIFIED_SOURCE ( 'ANY', '', #11473, .NOT_KNOWN. ) ;
#14168 = ORIENTED_EDGE ( 'NONE', *, *, #16859, .T. ) ;
#14169 = LINE ( 'NONE', #10054, #15300 ) ;
#14170 = ADVANCED_FACE ( 'NONE', ( #14952 ), #19304, .T. ) ;
#14171 = CARTESIAN_POINT ( 'NONE',  ( 42.63976443033212860, 50.99948385550240459, 0.02388180880522514787 ) ) ;
#14172 = EDGE_CURVE ( 'NONE', #5072, #1514, #15953, .T. ) ;
#14173 = EDGE_CURVE ( 'NONE', #164, #19088, #13195, .T. ) ;
#14174 = LINE ( 'NONE', #12813, #3724 ) ;
#14175 = ORIENTED_EDGE ( 'NONE', *, *, #14423, .T. ) ;
#14176 = ORIENTED_EDGE ( 'NONE', *, *, #13634, .T. ) ;
#14177 = DIRECTION ( 'NONE',  ( -0.000000000000000000, -1.000000000000000000, 8.673617379884036458E-16 ) ) ;
#14178 = EDGE_CURVE ( 'NONE', #1126, #728, #7408, .T. ) ;
#14179 = ORIENTED_EDGE ( 'NONE', *, *, #17483, .T. ) ;
#14180 = DIRECTION ( 'NONE',  ( 0.9989677110047502362, 0.04542589977017699732, -6.931730960091013400E-15 ) ) ;
#14181 = ORIENTED_EDGE ( 'NONE', *, *, #12926, .T. ) ;
#14182 = EDGE_CURVE ( 'NONE', #8777, #13296, #14559, .T. ) ;
#14183 = DIRECTION ( 'NONE',  ( -0.000000000000000000, -0.000000000000000000, 1.000000000000000000 ) ) ;
#14184 = DIRECTION ( 'NONE',  ( 0.000000000000000000, -1.000000000000000000, -0.000000000000000000 ) ) ;
#14185 = CARTESIAN_POINT ( 'NONE',  ( 43.69122665457040000, 62.00051614449766646, -0.02388180880515696977 ) ) ;
#14186 = DIRECTION ( 'NONE',  ( -1.000000000000000000, 0.000000000000000000, 0.000000000000000000 ) ) ;
#14187 = CARTESIAN_POINT ( 'NONE',  ( -29.99999999999999645, 0.000000000000000000, -10.00000000000000000 ) ) ;
#14188 = DIRECTION ( 'NONE',  ( 0.000000000000000000, -0.000000000000000000, 1.000000000000000000 ) ) ;
#14189 = AXIS2_PLACEMENT_3D ( 'NONE', #12404, #11026, #16933 ) ;
#14190 = ORIENTED_EDGE ( 'NONE', *, *, #8308, .T. ) ;
#14191 = ORIENTED_EDGE ( 'NONE', *, *, #1733, .T. ) ;
#14192 = LINE ( 'NONE', #4012, #7463 ) ;
#14193 = EDGE_CURVE ( 'NONE', #16121, #10087, #1238, .T. ) ;
#14194 = EDGE_CURVE ( 'NONE', #1029, #13080, #13288, .T. ) ;
#14195 = CARTESIAN_POINT ( 'NONE',  ( -154.9999999999999716, -14.99999999999999645, -15.00000000000000000 ) ) ;
#14196 = ITEM_DEFINED_TRANSFORMATION ( 'NONE', 'NONE', #16266,  #10359 ) ;
#14197 = ORIENTED_EDGE ( 'NONE', *, *, #5822, .T. ) ;
#14198 = DIRECTION ( 'NONE',  ( -0.5000000000000041078, 0.8660254037844362651, 0.000000000000000000 ) ) ;
#14199 = CARTESIAN_POINT ( 'NONE',  ( 75.00000000000001421, -2.999999999999999112, -5.999999999999998224 ) ) ;
#14200 = ORIENTED_EDGE ( 'NONE', *, *, #6749, .T. ) ;
#14201 = AXIS2_PLACEMENT_3D ( 'NONE', #2120, #6517, #9358 ) ;
#14202 = DIRECTION ( 'NONE',  ( 0.000000000000000000, 0.000000000000000000, 1.000000000000000000 ) ) ;
#14203 = DIRECTION ( 'NONE',  ( -0.000000000000000000, -0.000000000000000000, 1.000000000000000000 ) ) ;
#14204 = CARTESIAN_POINT ( 'NONE',  ( 6.534838248920897819, 2.951765777552411318, -5.112608298763837489 ) ) ;
#14205 = CIRCLE ( 'NONE', #12328, 20.00000000000000000 ) ;
#14206 = FACE_OUTER_BOUND ( 'NONE', #17295, .T. ) ;
#14207 = CARTESIAN_POINT ( 'NONE',  ( -14.17539641854911281, -34.10879641843998655, 0.000000000000000000 ) ) ;
#14208 = CARTESIAN_POINT ( 'NONE',  ( 45.86712807150323812, 65.29948385550241596, -5.649768623646098220 ) ) ;
#14209 = DIRECTION ( 'NONE',  ( -0.000000000000000000, -0.000000000000000000, 1.000000000000000000 ) ) ;
#14210 = CARTESIAN_POINT ( 'NONE',  ( 52.25172492374522903, 47.59948385550239891, -7.007379884777225953 ) ) ;
#14211 = CARTESIAN_POINT ( 'NONE',  ( 57.36023556966787851, 59.00051614449765935, 0.02388180880515038476 ) ) ;
#14212 = CARTESIAN_POINT ( 'NONE',  ( 2.449293598294706513E-15, -20.00000000000000000, 9.000000000000000000 ) ) ;
#14213 = CARTESIAN_POINT ( 'NONE',  ( 1.925929944387235853E-31, 15.00000000000001599, 9.000000000000000000 ) ) ;
#14214 = EDGE_CURVE ( 'NONE', #258, #7750, #2728, .T. ) ;
#14215 = EDGE_CURVE ( 'NONE', #12519, #14864, #10612, .T. ) ;
#14216 = VERTEX_POINT ( 'NONE', #1723 ) ;
#14217 = AXIS2_PLACEMENT_3D ( 'NONE', #19267, #214, #5806 ) ;
#14218 = CARTESIAN_POINT ( 'NONE',  ( 17.79870116617255604, -29.12174527145369396, 9.000000000000000000 ) ) ;
#14219 = EDGE_CURVE ( 'NONE', #1167, #11277, #2013, .T. ) ;
#14220 = DIRECTION ( 'NONE',  ( 0.000000000000000000, 0.000000000000000000, -1.000000000000000000 ) ) ;
#14221 = CARTESIAN_POINT ( 'NONE',  ( 52.29715082351539479, 54.60051614449766788, -6.992620115222796251 ) ) ;
#14222 = AXIS2_PLACEMENT_3D ( 'NONE', #8243, #18759, #3745 ) ;
#14223 = DIRECTION ( 'NONE',  ( 0.000000000000000000, 0.000000000000000000, 1.000000000000000000 ) ) ;
#14224 = DIRECTION ( 'NONE',  ( 1.000000000000000000, 0.000000000000000000, 0.000000000000000000 ) ) ;
#14225 = ORIENTED_EDGE ( 'NONE', *, *, #11412, .F. ) ;
#14226 = DIRECTION ( 'NONE',  ( -4.082155997157844188E-16, 1.000000000000000000, 0.000000000000000000 ) ) ;
#14227 = CARTESIAN_POINT ( 'NONE',  ( -2.915605589912154091E-15, 3.838309248099015747, 3.351853367131007566 ) ) ;
#14228 = LINE ( 'NONE', #4932, #5568 ) ;
#14229 = CARTESIAN_POINT ( 'NONE',  ( 49.97728705011488159, 45.49948385550240459, -7.000000000000000888 ) ) ;
#14230 = AXIS2_PLACEMENT_3D ( 'NONE', #4780, #170, #9081 ) ;
#14231 = CYLINDRICAL_SURFACE ( 'NONE', #8247, 1.000000000000000888 ) ;
#14232 = CARTESIAN_POINT ( 'NONE',  ( 52.62207051974839089, 48.39948385550240317, 7.992620115222770494 ) ) ;
#14233 = AXIS2_PLACEMENT_3D ( 'NONE', #8112, #10767, #17060 ) ;
#14234 = CARTESIAN_POINT ( 'NONE',  ( 44.28664221472221385, 63.90051614449765793, 1.832500667257213722 ) ) ;
#14235 = EDGE_CURVE ( 'NONE', #3923, #4718, #10529, .T. ) ;
#14236 = CYLINDRICAL_SURFACE ( 'NONE', #7868, 2.649999999999988365 ) ;
#14237 = DIRECTION ( 'NONE',  ( 1.000000000000000000, 0.000000000000000000, 0.000000000000000000 ) ) ;
#14238 = AXIS2_PLACEMENT_3D ( 'NONE', #9019, #15009, #6007 ) ;
#14239 = ORIENTED_EDGE ( 'NONE', *, *, #7841, .T. ) ;
#14240 = EDGE_CURVE ( 'NONE', #14289, #10053, #9064, .T. ) ;
#14241 = EDGE_LOOP ( 'NONE', ( #11922, #7798, #726, #3107 ) ) ;
#14242 = ORIENTED_EDGE ( 'NONE', *, *, #13361, .T. ) ;
#14243 = CARTESIAN_POINT ( 'NONE',  ( -19.97007065299860784, -21.09374499507130452, 0.000000000000000000 ) ) ;
#14244 = EDGE_LOOP ( 'NONE', ( #3436, #8288, #15928, #7096 ) ) ;
#14245 = FACE_OUTER_BOUND ( 'NONE', #1905, .T. ) ;
#14246 = ORIENTED_EDGE ( 'NONE', *, *, #10149, .T. ) ;
#14247 = DIRECTION ( 'NONE',  ( -0.3090169943749528914, 0.9510565162951518658, 0.000000000000000000 ) ) ;
#14248 = CARTESIAN_POINT ( 'NONE',  ( 55.94051828345050836, 57.79948385550240175, -4.345558710429103577 ) ) ;
#14249 = ORIENTED_EDGE ( 'NONE', *, *, #1860, .T. ) ;
#14250 = CARTESIAN_POINT ( 'NONE',  ( -9.999999999999994671, 20.00000000000001421, -9.999999999999998224 ) ) ;
#14251 = ORIENTED_EDGE ( 'NONE', *, *, #1780, .T. ) ;
#14252 = CARTESIAN_POINT ( 'NONE',  ( 43.18075615816989199, 55.19948385550240744, -4.924951120819313743 ) ) ;
#14253 = CARTESIAN_POINT ( 'NONE',  ( 3.974167765203684866, 0.7238254970431302615, -3.565825589389262085 ) ) ;
#14254 = AXIS2_PLACEMENT_3D ( 'NONE', #15372, #1952, #2142 ) ;
#14255 = CARTESIAN_POINT ( 'NONE',  ( 44.30067958973596376, 50.89948385550240317, 1.875703265242204099 ) ) ;
#14256 = CARTESIAN_POINT ( 'NONE',  ( 4.175326769692854434, 2.060699556488891027, -3.569236330973487803 ) ) ;
#14257 = CARTESIAN_POINT ( 'NONE',  ( 0.1717365941144614605, -6.008326913195983998, -0.8000000000000000444 ) ) ;
#14258 = CARTESIAN_POINT ( 'NONE',  ( 45.90387839640208512, 62.30051614449766362, -5.676469297603124353 ) ) ;
#14259 = CARTESIAN_POINT ( 'NONE',  ( 44.30067958973596376, 60.89948385550241028, 1.875703265242204099 ) ) ;
#14260 = VECTOR ( 'NONE', #13213, 1000.000000000000000 ) ;
#14261 = CARTESIAN_POINT ( 'NONE',  ( 56.65037692655918988, 59.89948385550241028, -2.184720259617163762 ) ) ;
#14262 = CARTESIAN_POINT ( 'NONE',  ( -6.259644161404860030E-16, -4.618802153517027165, -3.433295621305388234 ) ) ;
#14263 = CARTESIAN_POINT ( 'NONE',  ( -18.68843350152488725, -27.12337372732065077, -9.000000000000000000 ) ) ;
#14264 = VERTEX_POINT ( 'NONE', #441 ) ;
#14265 = ORIENTED_EDGE ( 'NONE', *, *, #11792, .F. ) ;
#14266 = CARTESIAN_POINT ( 'NONE',  ( 1.150000000000000577, 7.225416114969384193E-16, 5.899999999999999467 ) ) ;
#14267 = ORIENTED_EDGE ( 'NONE', *, *, #18591, .T. ) ;
#14268 = CARTESIAN_POINT ( 'NONE',  ( 57.36023556966787851, 59.99948385550240459, -0.02388180880522424582 ) ) ;
#14269 = CARTESIAN_POINT ( 'NONE',  ( 2.449293598294706513E-15, -20.00000000000000000, 9.000000000000000000 ) ) ;
#14270 = ORIENTED_EDGE ( 'NONE', *, *, #14292, .F. ) ;
#14271 = ORIENTED_EDGE ( 'NONE', *, *, #8915, .T. ) ;
#14272 = FACE_OUTER_BOUND ( 'NONE', #5864, .T. ) ;
#14273 = PRODUCT ( 'circlip for shafts normal_din_Circlip DIN 471 - 8 x 0.8', 'circlip for shafts normal_din_Circlip DIN 471 - 8 x 0.8', '', ( #14020 ) ) ;
#14274 = CIRCLE ( 'NONE', #9571, 0.7500000000000002220 ) ;
#14275 = ORIENTED_EDGE ( 'NONE', *, *, #7935, .F. ) ;
#14276 = CARTESIAN_POINT ( 'NONE',  ( 45.86712807150329496, 63.70051614449766220, 5.649768623646139964 ) ) ;
#14277 = ORIENTED_EDGE ( 'NONE', *, *, #9368, .F. ) ;
#14278 = DIRECTION ( 'NONE',  ( 0.000000000000000000, 0.000000000000000000, 1.000000000000000000 ) ) ;
#14279 = CARTESIAN_POINT ( 'NONE',  ( 4.000000000000000000, 0.000000000000000000, 0.000000000000000000 ) ) ;
#14280 = VECTOR ( 'NONE', #12574, 1000.000000000000000 ) ;
#14281 = CARTESIAN_POINT ( 'NONE',  ( 48.02776887271750184, 63.60051614449764656, 5.992620115222795363 ) ) ;
#14282 = DIRECTION ( 'NONE',  ( 0.000000000000000000, 0.000000000000000000, 1.000000000000000000 ) ) ;
#14283 = EDGE_CURVE ( 'NONE', #17307, #9631, #2168, .T. ) ;
#14284 = PLANE ( 'NONE',  #8008 ) ;
#14285 = CARTESIAN_POINT ( 'NONE',  ( -18.02113032590308705, -13.81966011250110249, -9.000000000000000000 ) ) ;
#14286 = PRODUCT_RELATED_PRODUCT_CATEGORY ( 'part', '', ( #4297 ) ) ;
#14287 = ADVANCED_FACE ( 'NONE', ( #3486 ), #2681, .F. ) ;
#14288 = PRODUCT_DEFINITION_SHAPE ( 'NONE', 'NONE',  #19421 ) ;
#14289 = VERTEX_POINT ( 'NONE', #10819 ) ;
#14290 = ORIENTED_EDGE ( 'NONE', *, *, #10216, .F. ) ;
#14291 = CARTESIAN_POINT ( 'NONE',  ( 4.197310751797292738, 0.8178363989516252985, -3.502498386812444409 ) ) ;
#14292 = EDGE_CURVE ( 'NONE', #17705, #6154, #9346, .T. ) ;
#14293 = EDGE_CURVE ( 'NONE', #8366, #8685, #3424, .T. ) ;
#14294 = VECTOR ( 'NONE', #2992, 1000.000000000000000 ) ;
#14295 = CARTESIAN_POINT ( 'NONE',  ( -160.9999999999999432, -14.99999999999999645, 6.499999999999999112 ) ) ;
#14296 = CARTESIAN_POINT ( 'NONE',  ( -32.00000000000000000, 3.000000000000000000, -5.999999999999998224 ) ) ;
#14297 = CONTEXT_DEPENDENT_SHAPE_REPRESENTATION ( #2289, #5531 ) ;
#14298 = ORIENTED_EDGE ( 'NONE', *, *, #16708, .T. ) ;
#14299 = CIRCLE ( 'NONE', #13982, 5.371010071662833063 ) ;
#14300 = DIRECTION ( 'NONE',  ( -0.000000000000000000, -0.000000000000000000, 1.000000000000000000 ) ) ;
#14301 = ADVANCED_FACE ( 'NONE', ( #1923 ), #11552, .T. ) ;
#14302 = ORIENTED_EDGE ( 'NONE', *, *, #9021, .T. ) ;
#14303 = CLOSED_SHELL ( 'NONE', ( #7737, #5378, #5560, #17096, #1175, #12764, #15381, #4416, #1741, #369, #7950, #5691, #19388, #3159, #19386, #13346, #17334, #15100, #2271, #10756, #11834, #3694 ) ) ;
#14304 = DIRECTION ( 'NONE',  ( 0.000000000000000000, 0.000000000000000000, 1.000000000000000000 ) ) ;
#14305 = CARTESIAN_POINT ( 'NONE',  ( 4.093692494532771953, 4.043567292011543302, -5.737475420082528345E-17 ) ) ;
#14306 = DIRECTION ( 'NONE',  ( -9.251858538542972814E-17, -1.000000000000000000, 0.000000000000000000 ) ) ;
#14307 = ADVANCED_FACE ( 'NONE', ( #12390 ), #4670, .F. ) ;
#14308 = CYLINDRICAL_SURFACE ( 'NONE', #1182, 0.9999999999999991118 ) ;
#14309 = ADVANCED_FACE ( 'NONE', ( #18212 ), #7888, .F. ) ;
#14310 = CARTESIAN_POINT ( 'NONE',  ( 46.49166364869460466, 50.69948385550240744, 4.867452303228209765 ) ) ;
#14311 = DIRECTION ( 'NONE',  ( -0.000000000000000000, 1.000000000000000000, 0.000000000000000000 ) ) ;
#14312 = CARTESIAN_POINT ( 'NONE',  ( 47.42335538002188144, 64.59948385550241312, 8.007379884777233059 ) ) ;
#14313 = CARTESIAN_POINT ( 'NONE',  ( 43.18075615816994173, 47.80051614449764941, 4.924951120819380357 ) ) ;
#14314 = FACE_OUTER_BOUND ( 'NONE', #4250, .T. ) ;
#14315 = DIRECTION ( 'NONE',  ( 0.000000000000000000, 0.000000000000000000, 1.000000000000000000 ) ) ;
#14316 = DIRECTION ( 'NONE',  ( 0.000000000000000000, 0.000000000000000000, -1.000000000000000000 ) ) ;
#14317 = AXIS2_PLACEMENT_3D ( 'NONE', #6376, #18461, #1981 ) ;
#14318 = ORIENTED_EDGE ( 'NONE', *, *, #15982, .F. ) ;
#14319 = DIRECTION ( 'NONE',  ( -0.000000000000000000, -0.000000000000000000, -1.000000000000000000 ) ) ;
#14320 = DIRECTION ( 'NONE',  ( 0.000000000000000000, -0.000000000000000000, 1.000000000000000000 ) ) ;
#14321 = AXIS2_PLACEMENT_3D ( 'NONE', #6219, #15231, #12095 ) ;
#14322 = CARTESIAN_POINT ( 'NONE',  ( 54.09612160359792199, 51.30051614449766362, 5.676469297603124353 ) ) ;
#14323 = CARTESIAN_POINT ( 'NONE',  ( 53.49409602498213445, 45.00000000000000711, -6.629536405711814240 ) ) ;
#14324 = CARTESIAN_POINT ( 'NONE',  ( 4.204015924366189871, -1.626724848190933548, -3.610627190413393084 ) ) ;
#14325 = ORIENTED_EDGE ( 'NONE', *, *, #10861, .F. ) ;
#14326 = CARTESIAN_POINT ( 'NONE',  ( 4.052424581287827010, -2.393186648133491357, 2.990837702970496892 ) ) ;
#14327 = CARTESIAN_POINT ( 'NONE',  ( -2.649999999999988365, 15.00000000000001599, 9.000000000000000000 ) ) ;
#14328 = CARTESIAN_POINT ( 'NONE',  ( -4.158233816355060064, -39.56295201467614220, -9.000000000000000000 ) ) ;
#14329 = CARTESIAN_POINT ( 'NONE',  ( 43.33558569842703179, 49.09948385550240602, -2.141517661632099223 ) ) ;
#14330 = CARTESIAN_POINT ( 'NONE',  ( 75.00000000000000000, 32.50000000000001421, -9.999999999999998224 ) ) ;
#14331 = CARTESIAN_POINT ( 'NONE',  ( 52.57664461997811856, 49.59948385550241312, -8.007379884777229506 ) ) ;
#14332 = CARTESIAN_POINT ( 'NONE',  ( 62.49999999999998579, 32.50000000000001421, 15.00000000000000000 ) ) ;
#14333 = MECHANICAL_DESIGN_GEOMETRIC_PRESENTATION_REPRESENTATION (  '', ( #18133 ), #15918 ) ;
#14334 = CARTESIAN_POINT ( 'NONE',  ( 50.02271294988505446, 44.50051614449765935, -7.000000000000000888 ) ) ;
#14335 = CIRCLE ( 'NONE', #6512, 4.000000000000000000 ) ;
#14336 = CARTESIAN_POINT ( 'NONE',  ( 1.149999999999998135, 0.000000000000000000, 0.000000000000000000 ) ) ;
#14337 = CARTESIAN_POINT ( 'NONE',  ( 4.050480423730738799, 1.376911654797411400, -3.567926555162023394 ) ) ;
#14338 = ORIENTED_EDGE ( 'NONE', *, *, #9143, .T. ) ;
#14339 = COLOUR_RGB ( '',0.8941176470588234615, 0.8941176470588234615, 0.8941176470588234615 ) ;
#14340 = ORIENTED_EDGE ( 'NONE', *, *, #5676, .T. ) ;
#14341 = FACE_OUTER_BOUND ( 'NONE', #365, .T. ) ;
#14342 = ORIENTED_EDGE ( 'NONE', *, *, #2477, .T. ) ;
#14343 = CARTESIAN_POINT ( 'NONE',  ( 6.244297270353399654, -0.9889575675955545320, 5.105276777067856209 ) ) ;
#14344 = ORIENTED_EDGE ( 'NONE', *, *, #17915, .T. ) ;
#14345 = CYLINDRICAL_SURFACE ( 'NONE', #4424, 0.9999999999999991118 ) ;
#14346 = CIRCLE ( 'NONE', #18755, 3.799999999999993605 ) ;
#14347 = CARTESIAN_POINT ( 'NONE',  ( 55.96859303347805081, 56.19948385550240744, 4.306917132069425058 ) ) ;
#14348 = EDGE_CURVE ( 'NONE', #5734, #1464, #10913, .T. ) ;
#14349 = CIRCLE ( 'NONE', #13117, 1.000000000000002665 ) ;
#14350 = ORIENTED_EDGE ( 'NONE', *, *, #1841, .F. ) ;
#14351 = CARTESIAN_POINT ( 'NONE',  ( 1.250000000000000000, -6.429618962271402616, -1.000000000000000000 ) ) ;
#14352 = VERTEX_POINT ( 'NONE', #6991 ) ;
#14353 = CARTESIAN_POINT ( 'NONE',  ( 52.57664461997811856, 59.59948385550240602, -8.007379884777229506 ) ) ;
#14354 = DIRECTION ( 'NONE',  ( -0.000000000000000000, -0.000000000000000000, 1.000000000000000000 ) ) ;
#14355 = EDGE_CURVE ( 'NONE', #10528, #5263, #308, .T. ) ;
#14356 = CARTESIAN_POINT ( 'NONE',  ( 55.11794222512601493, 48.19948385550240744, 3.688883143319541702 ) ) ;
#14357 = CARTESIAN_POINT ( 'NONE',  ( 5.991014884144047592, -4.330127018922191873, 2.499999999999998668 ) ) ;
#14358 = LINE ( 'NONE', #12600, #1816 ) ;
#14359 = STYLED_ITEM ( 'NONE', ( #6531 ), #14807 ) ;
#14360 = CARTESIAN_POINT ( 'NONE',  ( 56.81924384183006538, 46.80051614449766362, -4.924951120819380357 ) ) ;
#14361 = CARTESIAN_POINT ( 'NONE',  ( 50.02271294988506156, 44.50051614449765935, -6.000000000000000888 ) ) ;
#14362 = DIRECTION ( 'NONE',  ( -1.000000000000000000, -0.000000000000000000, -0.000000000000000000 ) ) ;
#14363 = CARTESIAN_POINT ( 'NONE',  ( -74.99999999999997158, 40.00000000000001421, 5.000000000000018652 ) ) ;
#14364 = ORIENTED_EDGE ( 'NONE', *, *, #15493, .T. ) ;
#14365 = CIRCLE ( 'NONE', #1876, 5.575000000000000178 ) ;
#14366 = ORIENTED_EDGE ( 'NONE', *, *, #18497, .F. ) ;
#14367 = PLANE ( 'NONE',  #17196 ) ;
#14368 = FILL_AREA_STYLE ('',( #11038 ) ) ;
#14369 = ORIENTED_EDGE ( 'NONE', *, *, #17583, .T. ) ;
#14370 = CARTESIAN_POINT ( 'NONE',  ( 47.70284917648453415, 59.39948385550241028, -6.992620115222774047 ) ) ;
#14371 = FACE_OUTER_BOUND ( 'NONE', #16959, .T. ) ;
#14372 = ORIENTED_EDGE ( 'NONE', *, *, #1256, .T. ) ;
#14373 = ORIENTED_EDGE ( 'NONE', *, *, #13865, .T. ) ;
#14374 = DIRECTION ( 'NONE',  ( 1.000000000000000000, 0.000000000000000000, 0.000000000000000000 ) ) ;
#14375 = ORIENTED_EDGE ( 'NONE', *, *, #16204, .T. ) ;
#14376 = CARTESIAN_POINT ( 'NONE',  ( 0.000000000000000000, 0.000000000000000000, -0.8000000000000000444 ) ) ;
#14377 = VERTEX_POINT ( 'NONE', #3575 ) ;
#14378 = AXIS2_PLACEMENT_3D ( 'NONE', #16031, #14451, #11207 ) ;
#14379 = VECTOR ( 'NONE', #687, 1000.000000000000000 ) ;
#14380 = B_SPLINE_CURVE_WITH_KNOTS ( 'NONE', 3,
 ( #11680, #16403, #4536, #3072, #3169, #10495, #10594, #2970, #15115, #13547, #1491, #13251, #5805, #7467, #120, #12069 ),
 .UNSPECIFIED., .F., .F.,
 ( 4, 3, 3, 3, 3, 4 ),
 ( 0.000000000000000000, 5.303647860849292387E-05, 0.0001057093501027219331, 0.0001642058037231606204, 0.0002210073443958821807, 0.0002236769549542877021 ),
 .UNSPECIFIED. ) ;
#14381 = CARTESIAN_POINT ( 'NONE',  ( 57.36023556966787851, 53.99948385550239038, -0.02388180880522424582 ) ) ;
#14382 = LINE ( 'NONE', #5082, #4290 ) ;
#14383 = CARTESIAN_POINT ( 'NONE',  ( 42.63976443033212860, 48.00051614449766646, -0.02388180880514948964 ) ) ;
#14384 = DIRECTION ( 'NONE',  ( -0.000000000000000000, -0.000000000000000000, -1.000000000000000000 ) ) ;
#14385 = PLANE ( 'NONE',  #4570 ) ;
#14386 = AXIS2_PLACEMENT_3D ( 'NONE', #13056, #2880, #17876 ) ;
#14387 = LINE ( 'NONE', #6741, #15666 ) ;
#14388 = ORIENTED_EDGE ( 'NONE', *, *, #8713, .T. ) ;
#14389 = ORIENTED_EDGE ( 'NONE', *, *, #3944, .T. ) ;
#14390 = CARTESIAN_POINT ( 'NONE',  ( 4.050823680195223098, 2.400527758044901372, 2.978030508226146900 ) ) ;
#14391 = AXIS2_PLACEMENT_3D ( 'NONE', #5307, #14220, #8047 ) ;
#14392 = CARTESIAN_POINT ( 'NONE',  ( -155.0676494111543491, -18.79939778875158396, -15.00000000000000000 ) ) ;
#14393 = DIRECTION ( 'NONE',  ( 1.000000000000000000, 0.000000000000000000, 0.000000000000000000 ) ) ;
#14394 = ORIENTED_EDGE ( 'NONE', *, *, #7011, .T. ) ;
#14395 = LINE ( 'NONE', #4017, #17416 ) ;
#14396 = ADVANCED_FACE ( 'NONE', ( #9927 ), #12586, .T. ) ;
#14397 = AXIS2_PLACEMENT_3D ( 'NONE', #8382, #2631, #5356 ) ;
#14398 = ORIENTED_EDGE ( 'NONE', *, *, #2019, .F. ) ;
#14399 = ORIENTED_EDGE ( 'NONE', *, *, #18185, .T. ) ;
#14400 = CARTESIAN_POINT ( 'NONE',  ( -20.63749999999999929, 0.000000000000000000, 0.000000000000000000 ) ) ;
#14401 = DIRECTION ( 'NONE',  ( 0.000000000000000000, 0.000000000000000000, 1.000000000000000000 ) ) ;
#14402 = APPLICATION_CONTEXT ( 'automotive_design' ) ;
#14404 = CIRCLE ( 'NONE', #5638, 2.649999999999985700 ) ;
#14403 = CARTESIAN_POINT ( 'NONE',  ( 43.69122665457040000, 62.99948385550241170, 0.02388180880521036456 ) ) ;
#14405 = DIRECTION ( 'NONE',  ( 1.000000000000000000, 0.000000000000000000, 0.000000000000000000 ) ) ;
#14406 = CARTESIAN_POINT ( 'NONE',  ( 0.2182387239031248760, 1.693823289467350168, 3.500000000000000000 ) ) ;
#14407 = CARTESIAN_POINT ( 'NONE',  ( 53.50833635130540955, 51.69948385550241454, -4.867452303228209765 ) ) ;
#14408 = AXIS2_PLACEMENT_3D ( 'NONE', #4199, #8703, #6065 ) ;
#14409 = CARTESIAN_POINT ( 'NONE',  ( 0.1481481481481481122, -4.797713218419819903, -1.000000000000000000 ) ) ;
#14410 = AXIS2_PLACEMENT_3D ( 'NONE', #4863, #2114, #10824 ) ;
#14411 = CARTESIAN_POINT ( 'NONE',  ( 54.09612160359786515, 45.69948385550240744, -5.676469297603166098 ) ) ;
#14412 = CARTESIAN_POINT ( 'NONE',  ( 52.62207051974829852, 44.60051614449766078, -7.992620115222797139 ) ) ;
#14413 = EDGE_CURVE ( 'NONE', #5527, #4462, #18788, .T. ) ;
#14414 = AXIS2_PLACEMENT_3D ( 'NONE', #10311, #5722, #35 ) ;
#14415 = CARTESIAN_POINT ( 'NONE',  ( 10.00000000000000000, 15.00000000000001776, 15.00000000000000000 ) ) ;
#14416 = FACE_OUTER_BOUND ( 'NONE', #1571, .T. ) ;
#14417 = B_SPLINE_CURVE_WITH_KNOTS ( 'NONE', 3,
 ( #13915, #12272, #17176, #6572, #18368, #4915, #3735, #10788 ),
 .UNSPECIFIED., .F., .F.,
 ( 4, 2, 2, 4 ),
 ( 0.000000000000000000, 0.001493104274552339720, 0.002986208549104679439, 0.005972417098209361480 ),
 .UNSPECIFIED. ) ;
#14418 = DIRECTION ( 'NONE',  ( 1.000000000000000000, 0.000000000000000000, 0.000000000000000000 ) ) ;
#14419 = EDGE_LOOP ( 'NONE', ( #6722, #6822, #43, #15476 ) ) ;
#14420 = AXIS2_PLACEMENT_3D ( 'NONE', #15983, #11654, #2573 ) ;
#14421 = LINE ( 'NONE', #6972, #4871 ) ;
#14422 = ADVANCED_FACE ( 'NONE', ( #17211 ), #18495, .F. ) ;
#14423 = EDGE_CURVE ( 'NONE', #8944, #10636, #9827, .T. ) ;
#14424 = CARTESIAN_POINT ( 'NONE',  ( 2.059999999999998721, 0.000000000000000000, -0.3080913168122742518 ) ) ;
#14425 = AXIS2_PLACEMENT_3D ( 'NONE', #8091, #16846, #10937 ) ;
#14426 = AXIS2_PLACEMENT_3D ( 'NONE', #15667, #11046, #13980 ) ;
#14427 = VECTOR ( 'NONE', #5223, 1000.000000000000000 ) ;
#14428 = CARTESIAN_POINT ( 'NONE',  ( 42.63976443033212149, 56.00051614449765225, -0.02388180880514948964 ) ) ;
#14429 = FACE_OUTER_BOUND ( 'NONE', #13949, .T. ) ;
#14430 = DIRECTION ( 'NONE',  ( 0.000000000000000000, -0.000000000000000000, 1.000000000000000000 ) ) ;
#14431 = VERTEX_POINT ( 'NONE', #12784 ) ;
#14432 = CARTESIAN_POINT ( 'NONE',  ( 3.958484000407985981, -2.327740518749076948, 2.968235154689861321 ) ) ;
#14433 = CARTESIAN_POINT ( 'NONE',  ( 2.000000000000000000, -0.8865213383406694847, 1.535500000000001419 ) ) ;
#14434 = EDGE_CURVE ( 'NONE', #8760, #15486, #2110, .T. ) ;
#14435 = FACE_OUTER_BOUND ( 'NONE', #17020, .T. ) ;
#14436 = CARTESIAN_POINT ( 'NONE',  ( 52.25172492374522903, 51.59948385550240602, -7.007379884777225953 ) ) ;
#14437 = ADVANCED_FACE ( 'NONE', ( #8070, #15828, #923 ), #629, .T. ) ;
#14438 = DIRECTION ( 'NONE',  ( -2.191393683118470056E-17, -7.538405132783724027E-17, -1.000000000000000000 ) ) ;
#14439 = CARTESIAN_POINT ( 'NONE',  ( 57.60143344285433642, 45.89948385550240317, -2.493737253992118319 ) ) ;
#14440 = CARTESIAN_POINT ( 'NONE',  ( -160.9999999999999432, -14.99999999999999645, 6.499999999999999112 ) ) ;
#14441 = CARTESIAN_POINT ( 'NONE',  ( 49.97728705011495265, 51.50051614449765935, 7.000000000000000888 ) ) ;
#14442 = EDGE_CURVE ( 'NONE', #16376, #7688, #5926, .T. ) ;
#14443 = CARTESIAN_POINT ( 'NONE',  ( -54.99999999999996447, -22.99999999999998579, 15.00000000000000000 ) ) ;
#14444 = AXIS2_PLACEMENT_3D ( 'NONE', #3493, #7896, #15640 ) ;
#14445 = DIRECTION ( 'NONE',  ( -0.000000000000000000, -0.000000000000000000, -1.000000000000000000 ) ) ;
#14446 = ORIENTED_EDGE ( 'NONE', *, *, #186, .F. ) ;
#14447 = MECHANICAL_DESIGN_GEOMETRIC_PRESENTATION_REPRESENTATION (  '', ( #19185 ), #1318 ) ;
#14448 = EDGE_LOOP ( 'NONE', ( #13802, #14512 ) ) ;
#14449 = DIRECTION ( 'NONE',  ( -1.734723475976807341E-16, -1.000000000000000000, 0.000000000000000000 ) ) ;
#14450 = EDGE_LOOP ( 'NONE', ( #7601, #3603, #16134, #18166 ) ) ;
#14451 = DIRECTION ( 'NONE',  ( -9.858538378746663627E-23, 5.031452844637890958E-23, -1.000000000000000000 ) ) ;
#14452 = ORIENTED_EDGE ( 'NONE', *, *, #8720, .F. ) ;
#14453 = DIRECTION ( 'NONE',  ( 0.000000000000000000, 0.000000000000000000, 1.000000000000000000 ) ) ;
#14454 = CARTESIAN_POINT ( 'NONE',  ( 47.70284917648453415, 59.39948385550241028, -6.992620115222774047 ) ) ;
#14455 = ORIENTED_EDGE ( 'NONE', *, *, #17138, .F. ) ;
#14456 = CARTESIAN_POINT ( 'NONE',  ( -4.872650870659752442, 0.4273491293402474911, -0.8000000000000000444 ) ) ;
#14457 = ORIENTED_EDGE ( 'NONE', *, *, #3350, .F. ) ;
#14458 = CARTESIAN_POINT ( 'NONE',  ( 42.38452918213188525, 59.09948385550240602, -2.450534656007040013 ) ) ;
#14459 = CARTESIAN_POINT ( 'NONE',  ( 1.000000000000002442, -20.00000000000000000, -9.000000000000001776 ) ) ;
#14460 = PRODUCT_DEFINITION_SHAPE ( 'NONE', 'NONE',  #1359 ) ;
#14461 = CARTESIAN_POINT ( 'NONE',  ( 48.07319477248768180, 50.59948385550240602, 6.007379884777225953 ) ) ;
#14462 = DIRECTION ( 'NONE',  ( 1.000000000000000000, 0.000000000000000000, 0.000000000000000000 ) ) ;
#14463 = AXIS2_PLACEMENT_3D ( 'NONE', #791, #17732, #695 ) ;
#14464 = CARTESIAN_POINT ( 'NONE',  ( -19.99999999999999645, -20.00000000000000000, -9.000000000000000000 ) ) ;
#14465 = CARTESIAN_POINT ( 'NONE',  ( 57.60143344285435774, 49.10051614449766788, 2.493737253992045044 ) ) ;
#14466 = CARTESIAN_POINT ( 'NONE',  ( 44.91013252490150620, 48.20051614449766930, -3.727524721679154940 ) ) ;
#14467 = CARTESIAN_POINT ( 'NONE',  ( 6.534533895392292457, -2.951347675328713116, 5.111884124469662893 ) ) ;
#14468 = FACE_OUTER_BOUND ( 'NONE', #16557, .T. ) ;
#14469 = ORIENTED_EDGE ( 'NONE', *, *, #7486, .F. ) ;
#14470 = ADVANCED_FACE ( 'NONE', ( #8362 ), #17405, .F. ) ;
#14471 = VERTEX_POINT ( 'NONE', #18785 ) ;
#14472 = CARTESIAN_POINT ( 'NONE',  ( -154.9999999999999716, -23.00000000000000000, -15.00000000000000000 ) ) ;
#14473 = ORIENTED_EDGE ( 'NONE', *, *, #11062, .T. ) ;
#14474 = EDGE_CURVE ( 'NONE', #13579, #18552, #13130, .T. ) ;
#14475 = CARTESIAN_POINT ( 'NONE',  ( 54.09612160359786515, 59.69948385550240033, -5.676469297603166098 ) ) ;
#14476 = FILL_AREA_STYLE_COLOUR ( '', #19086 ) ;
#14477 = VERTEX_POINT ( 'NONE', #2411 ) ;
#14478 = ORIENTED_EDGE ( 'NONE', *, *, #10953, .F. ) ;
#14479 = DIRECTION ( 'NONE',  ( 0.9135454576426006446, 0.4067366430758008189, 0.000000000000000000 ) ) ;
#14480 = EDGE_LOOP ( 'NONE', ( #17193, #1953, #18394, #3866 ) ) ;
#14481 = DIRECTION ( 'NONE',  ( 1.000000000000000000, 0.000000000000000000, 0.000000000000000000 ) ) ;
#14482 = ORIENTED_EDGE ( 'NONE', *, *, #9868, .F. ) ;
#14483 = CARTESIAN_POINT ( 'NONE',  ( 43.33558569842703179, 49.09948385550240602, -2.141517661632099223 ) ) ;
#14484 = DIRECTION ( 'NONE',  ( -1.000000000000000000, 0.000000000000000000, 0.000000000000000000 ) ) ;
#14485 = CARTESIAN_POINT ( 'NONE',  ( 52.29715082351538769, 50.60051614449766788, -6.992620115222796251 ) ) ;
#14486 = DIRECTION ( 'NONE',  ( 0.000000000000000000, 0.000000000000000000, 1.000000000000000000 ) ) ;
#14487 = CARTESIAN_POINT ( 'NONE',  ( -62.49999999999997158, 20.00000000000001421, 9.999999999999998224 ) ) ;
#14488 = PRODUCT_DEFINITION_FORMATION_WITH_SPECIFIED_SOURCE ( 'ANY', '', #16350, .NOT_KNOWN. ) ;
#14489 = CARTESIAN_POINT ( 'NONE',  ( 0.000000000000000000, 0.000000000000000000, 2.500000000000000444 ) ) ;
#14490 = ORIENTED_EDGE ( 'NONE', *, *, #13395, .F. ) ;
#14491 = ORIENTED_EDGE ( 'NONE', *, *, #6215, .F. ) ;
#14492 = CARTESIAN_POINT ( 'NONE',  ( -62.49999999999997158, 45.00000000000001421, 15.00000000000000000 ) ) ;
#14493 = CARTESIAN_POINT ( 'NONE',  ( -4.078421086530219064, -3.990950201428956845, -1.000000000000000000 ) ) ;
#14494 = SURFACE_SIDE_STYLE ('',( #10082 ) ) ;
#14495 = EDGE_LOOP ( 'NONE', ( #7536, #18494, #3961 ) ) ;
#14496 = CARTESIAN_POINT ( 'NONE',  ( 3.129923130707922496, -23.63917314727666152, -8.999999999999996447 ) ) ;
#14497 = ORIENTED_EDGE ( 'NONE', *, *, #10705, .T. ) ;
#14498 = ORIENTED_EDGE ( 'NONE', *, *, #19262, .F. ) ;
#14499 = DIRECTION ( 'NONE',  ( -1.000000000000000000, 0.000000000000000000, 0.000000000000000000 ) ) ;
#14500 = FACE_OUTER_BOUND ( 'NONE', #13799, .T. ) ;
#14501 = CARTESIAN_POINT ( 'NONE',  ( 44.28664221472221385, 47.90051614449765793, 1.832500667257213722 ) ) ;
#14502 = DIRECTION ( 'NONE',  ( 0.000000000000000000, 0.5000000000000018874, 0.8660254037844375974 ) ) ;
#14503 = DIRECTION ( 'NONE',  ( 0.000000000000000000, 0.000000000000000000, 1.000000000000000000 ) ) ;
#14504 = CARTESIAN_POINT ( 'NONE',  ( 44.28664221472220675, 53.09948385550240602, -1.832500667257165317 ) ) ;
#14505 = LINE ( 'NONE', #11461, #6319 ) ;
#14506 = CARTESIAN_POINT ( 'NONE',  ( 47.70284917648453415, 47.39948385550238896, -6.992620115222774047 ) ) ;
#14507 = CARTESIAN_POINT ( 'NONE',  ( 52.62207051974829852, 48.60051614449766788, -7.992620115222797139 ) ) ;
#14508 = CARTESIAN_POINT ( 'NONE',  ( -3.333333333333332149, -2.694301256218264218, -3.300726591567082036 ) ) ;
#14509 = DIRECTION ( 'NONE',  ( 0.000000000000000000, 0.000000000000000000, -1.000000000000000000 ) ) ;
#14510 =( NAMED_UNIT ( * ) PLANE_ANGLE_UNIT ( ) SI_UNIT ( $, .RADIAN. ) );
#14511 = DIRECTION ( 'NONE',  ( 1.000000000000000000, 0.000000000000000000, 0.000000000000000000 ) ) ;
#14512 = ORIENTED_EDGE ( 'NONE', *, *, #17298, .T. ) ;
#14513 = CARTESIAN_POINT ( 'NONE',  ( -1.390230914382372118, -4.043987460488664532, -3.502507215260523665 ) ) ;
#14514 = VECTOR ( 'NONE', #11117, 999.9999999999998863 ) ;
#14515 = CARTESIAN_POINT ( 'NONE',  ( -13.86289650954791064, -6.617387872822862782, 9.000000000000000000 ) ) ;
#14516 = CARTESIAN_POINT ( 'NONE',  ( 55.96859303347802239, 50.80051614449766362, -4.306917132069484566 ) ) ;
#14517 = DIRECTION ( 'NONE',  ( -0.000000000000000000, -0.000000000000000000, -1.000000000000000000 ) ) ;
#14518 = CARTESIAN_POINT ( 'NONE',  ( -62.49999999999997158, 32.50000000000001421, 9.999999999999998224 ) ) ;
#14519 = ORIENTED_EDGE ( 'NONE', *, *, #7602, .F. ) ;
#14520 = CARTESIAN_POINT ( 'NONE',  ( -155.0777214229742071, -18.79920509849242549, 15.79999999999999893 ) ) ;
#14521 = DIRECTION ( 'NONE',  ( 1.000000000000000000, -9.251858538542972814E-17, 0.000000000000000000 ) ) ;
#14522 = CARTESIAN_POINT ( 'NONE',  ( 55.96859303347804371, 50.19948385550240744, 4.306917132069425946 ) ) ;
#14523 = FACE_OUTER_BOUND ( 'NONE', #18012, .T. ) ;
#14524 = CARTESIAN_POINT ( 'NONE',  ( 52.57664461997811856, 47.59948385550239891, -8.007379884777229506 ) ) ;
#14525 = ADVANCED_FACE ( 'NONE', ( #14341 ), #729, .T. ) ;
#14526 = CARTESIAN_POINT ( 'NONE',  ( 44.03140696652198471, 47.80051614449764230, 4.306917132069485454 ) ) ;
#14527 = CYLINDRICAL_SURFACE ( 'NONE', #15038, 1.000000000000000000 ) ;
#14528 = AXIS2_PLACEMENT_3D ( 'NONE', #9028, #1692, #13449 ) ;
#14529 = VERTEX_POINT ( 'NONE', #3963 ) ;
#14530 = ADVANCED_FACE ( 'NONE', ( #18686 ), #18885, .F. ) ;
#14531 = EDGE_LOOP ( 'NONE', ( #7507, #9196, #7691, #4621 ) ) ;
#14532 = CARTESIAN_POINT ( 'NONE',  ( 2.449293598294706513E-15, -20.00000000000000000, 9.000000000000000000 ) ) ;
#14533 = ORIENTED_EDGE ( 'NONE', *, *, #2351, .T. ) ;
#14534 = EDGE_CURVE ( 'NONE', #6336, #12413, #10303, .T. ) ;
#14535 = EDGE_CURVE ( 'NONE', #5652, #3609, #8264, .T. ) ;
#14536 = PLANE ( 'NONE',  #3128 ) ;
#14537 = EDGE_LOOP ( 'NONE', ( #12401, #1749, #13071, #13841 ) ) ;
#14538 = CARTESIAN_POINT ( 'NONE',  ( 4.000000000000000000, 2.309401076758497151, -3.433295621305379353 ) ) ;
#14539 = EDGE_CURVE ( 'NONE', #19337, #13491, #5044, .T. ) ;
#14540 = VERTEX_POINT ( 'NONE', #4720 ) ;
#14541 = DIRECTION ( 'NONE',  ( -0.000000000000000000, -0.000000000000000000, 1.000000000000000000 ) ) ;
#14542 = ORIENTED_EDGE ( 'NONE', *, *, #19355, .F. ) ;
#14543 = CARTESIAN_POINT ( 'NONE',  ( 47.42335538002188144, 56.59948385550239891, 8.007379884777233059 ) ) ;
#14544 = AXIS2_PLACEMENT_3D ( 'NONE', #3712, #12628, #6838 ) ;
#14545 = DIRECTION ( 'NONE',  ( -1.000000000000000000, -0.000000000000000000, -0.000000000000000000 ) ) ;
#14546 = CARTESIAN_POINT ( 'NONE',  ( 48.02776887271745210, 53.39948385550241028, -5.992620115222778487 ) ) ;
#14547 = CARTESIAN_POINT ( 'NONE',  ( 0.000000000000000000, 0.000000000000000000, 0.000000000000000000 ) ) ;
#14548 = DIRECTION ( 'NONE',  ( 0.000000000000000000, 0.000000000000000000, -1.000000000000000000 ) ) ;
#14549 = CARTESIAN_POINT ( 'NONE',  ( 42.38452918213190657, 47.90051614449765793, 2.450534656007115508 ) ) ;
#14550 = VECTOR ( 'NONE', #14319, 1000.000000000000000 ) ;
#14551 = ADVANCED_FACE ( 'NONE', ( #16216 ), #7189, .F. ) ;
#14552 = CARTESIAN_POINT ( 'NONE',  ( 44.91013252490150620, 50.20051614449766220, -3.727524721679154940 ) ) ;
#14553 = EDGE_CURVE ( 'NONE', #15764, #16268, #14365, .T. ) ;
#14554 = CARTESIAN_POINT ( 'NONE',  ( -3.264650091097280831E-13, -4.796980096169642493, -3.721999068284424617 ) ) ;
#14555 = DIRECTION ( 'NONE',  ( -0.9989677110047502362, -0.04542589977017699732, 6.931730960091013400E-15 ) ) ;
#14556 = ORIENTED_EDGE ( 'NONE', *, *, #8089, .T. ) ;
#14557 =( BOUNDED_SURFACE ( )  B_SPLINE_SURFACE ( 3, 2, ( 
 ( #14229, #15521, #17012, #17300, #9439, #17199, #9817, #12379, #2098, #2004, #9623, #12578, #14134, #7966, #3856, #6492, #11006, #8057, #3756, #13938, #15720, #15618, #618, #18586, #18388, #11094, #12772, #2197, #10904, #2300, #8254, #815, #18773, #11292, #11773, #7079, #14329, #913, #14722, #1309, #8555, #16113, #2398, #9915, #2692, #1018, #19070, #14522, #6980, #12960, #8351, #16206, #5809, #11386, #1205, #5716, #8646, #6881, #18968, #5612, #19175, #14436, #17394, #1108, #19270, #15914, #5509, #11482, #13254, #17491, #3954, #18874, #11585, #13062, #4053, #10015, #2501, #13159, #5413, #8745, #16018, #2603, #17778, #8455, #11683, #4337, #12872, #17597, #4151, #2783, #10116, #17686, #7278, #10305, #14619, #7180, #4239, #10202, #13735, #18269, #321, #4539, #4824, #19369, #11977, #16311, #2885, #3173, #10406, #12170, #8845, #29, #6197, #18178, #14821, #9032, #6296, #18074, #1497, #13451, #17981, #1401, #7377, #13349, #216, #10498, #12271, #15019, #7661, #7470, #13642, #9134, #16502, #17881, #6015, #4736, #15118, #5904, #11873, #14921, #6103, #3076, #15212, #9222, #10697, #4638, #1694, #1598, #1789, #7568, #4446, #16406, #2973, #13550, #16601, #7760, #8938, #123, #16697, #12073, #10597, #3261, #16890, #3638, #12653, #3547, #413, #1982, #7946, #13914, #3734, #2280, #9597, #14114, #18660, #6571, #12452, #15496, #5008, #15405, #6671, #18565, #8233, #501, #4914, #6377, #3453, #18462, #796, #10985, #6472, #16992, #9506, #11166, #2074, #10884, #5197, #6767, #14208, #8035, #12357 ),
 ( #14011, #2175, #15595, #596, #18367, #12558, #17174, #5107, #9418, #11077, #17082, #8137, #700, #12750, #9700, #15701, #18746, #10787, #16790, #3356, #9318, #15307, #1888, #7859, #13832, #4217, #6857, #3838, #1187, #8330, #11265, #18854, #10184, #14698, #9993, #17278, #9799, #17662, #16184, #11460, #19047, #5293, #12844, #5590, #3935, #2581, #17471, #9893, #15893, #15795, #19149, #8724, #14310, #4128, #8626, #11560, #5395, #888, #11367, #6962, #1287, #12941, #14407, #18950, #2478, #5695, #4030, #17374, #13139, #7261, #13235, #5490, #8430, #995, #11661, #1089, #14504, #2376, #2765, #7059, #8534, #15990, #13040, #17574, #10095, #16090, #14599, #2673, #7160, #16388, #1378, #10387, #2953, #2862, #7739, #17962, #16483, #1473, #14996, #19245, #106, #5993, #4615, #1577, #12055, #1768, #12149, #8918, #17860, #19345, #7549, #18054, #200, #4422, #4520, #13534, #3052, #10479, #5886, #6177, #5787, #10574, #9011, #9115, #11959, #13325, #16578, #7352, #18153, #6084, #3149, #15102, #11751, #7451, #11853, #14899, #1679, #17758, #16680, #13432, #7642, #13622, #4712, #10675, #3246, #9205, #15191, #7, #4317, #10286, #16289, #8826, #14799, #6718, #14259, #12902, #2533, #17228, #17329, #296, #11124, #3793, #394, #6818, #15843, #12701, #3336, #5151, #17130, #3689, #6916, #5442, #12804, #3887, #2428, #9757, #15650, #18704, #8193, #18611, #9843, #2328, #11419, #9653, #12247, #8380, #16771, #6268, #7833, #18904, #3980, #5250, #18252, #4808, #17421, #9944, #744, #8281, #13717, #1867, #842 ),
 ( #14361, #15943, #9297, #18804, #945, #5354, #10771, #12602, #15750, #11326, #6362, #15287, #11221, #13811, #2235, #14161, #17625, #19400, #4175, #4082, #5536, #11706, #14647, #19098, #5639, #16047, #19299, #11511, #14852, #10141, #16144, #17910, #10049, #5836, #10430, #1046, #2629, #14466, #8870, #17713, #4367, #1430, #7403, #2909, #7012, #11615, #12991, #5938, #16434, #11900, #2721, #8490, #17521, #8676, #18998, #8583, #14750, #14552, #10331, #1136, #1233, #17811, #16337, #7107, #7206, #4469, #10235, #13089, #13190, #19203, #5742, #4269, #16236, #11806, #2810, #8772, #1334, #13377, #7308, #13283, #15233, #18103, #4566, #7592, #10810, #4664, #10525, #18205, #1717, #3282, #16529, #18390, #1631, #13572, #6127, #7783, #3102, #16814, #4762, #146, #15139, #4936, #10623, #1915, #9058, #7685, #9245, #7881, #10907, #6222, #6321, #8962, #12097, #12195, #15049, #1813, #4849, #13665, #12001, #16630, #3199, #9161, #15334, #13854, #13761, #12294, #3377, #10722, #240, #16721, #346, #18294, #9340, #434, #6404, #12383, #3003, #18006, #14945, #1525, #7499, #13481, #57, #6037, #14037, #17304, #15622, #17017, #5323, #6888, #917, #5128, #12475, #622, #11298, #12678, #6693, #2007, #3861, #18679, #14137, #3479, #18488, #12581, #5222, #9821, #820, #9627, #8062, #6599, #5037, #18590, #11099, #523, #5417, #2202, #723, #17106, #11196, #16915, #17202, #3664, #2304, #3760, #9727, #18879, #15822, #8164, #15525, #3567, #15723, #8257, #2403, #2101, #14234, #6790, #12776, #18777, #9533, #8356, #9443 ),
 ( #14334, #15428, #12876, #7970, #6496, #13942, #11009, #5721, #11390, #10020, #14622, #8749, #4057, #6985, #4156, #8850, #18973, #8561, #1112, #2890, #7083, #12964, #8460, #1209, #17600, #2608, #10120, #11686, #10309, #19374, #7184, #14727, #17400, #14526, #13164, #17495, #4244, #13259, #16117, #1022, #13066, #19074, #5616, #4341, #14826, #10207, #1312, #19274, #19180, #11590, #2697, #8650, #16021, #7283, #17690, #1405, #16210, #5513, #11486, #2788, #5813, #7381, #11779, #17783, #16315, #13354, #3958, #9920, #15920, #2505, #14441, #9321, #13554, #1501, #9036, #13739, #1698, #15122, #10411, #324, #7665, #3178, #11877, #7475, #1604, #13646, #6300, #9225, #18079, #16507, #3080, #13456, #15024, #7572, #8942, #13835, #4642, #9139, #127, #221, #5910, #6201, #12077, #10702, #12175, #18182, #7862, #18273, #6107, #4543, #6019, #4741, #16701, #12274, #10502, #10603, #3264, #15215, #16605, #11981, #4828, #17886, #1794, #7763, #10790, #16793, #34, #3359, #17985, #15310, #1891, #4450, #16410, #2977, #14926, #505, #12455, #12656, #12361, #17281, #18466, #9601, #6575, #18750, #12753, #14211, #8142, #5200, #5011, #5297, #2077, #3841, #9422, #18370, #15408, #12561, #9802, #7949, #16995, #9509, #11271, #15499, #1985, #16894, #3641, #18568, #10988, #3550, #13917, #11170, #3456, #6770, #8040, #14015, #15798, #6476, #17178, #2379, #4918, #600, #6381, #799, #15599, #15704, #8333, #416, #10887, #5110, #11080, #17085, #2179, #14117, #703, #6674, #18663, #3739, #9704, #2283, #8237, #1191, #8434 ),
 ( #13043, #14412, #2769, #4321, #17761, #2584, #9896, #17475, #8727, #10098, #4131, #18857, #14702, #16093, #11564, #891, #15897, #9997, #2676, #1292, #17665, #7062, #5493, #11463, #2481, #4034, #15995, #17377, #2866, #19051, #17579, #8537, #8629, #14313, #14602, #1092, #19155, #7163, #13143, #16293, #7265, #14507, #12944, #998, #5698, #11664, #13238, #18953, #5594, #4220, #10187, #16187, #6965, #19248, #6861, #5790, #11754, #10289, #12849, #5398, #11370, #3938, #7741, #1580, #6180, #3152, #8829, #10482, #8921, #1476, #1681, #1382, #6271, #7454, #16774, #7553, #6087, #16485, #4617, #14803, #9118, #14999, #13625, #10576, #7645, #10773, #1770, #5999, #13435, #14902, #16580, #202, #9208, #11, #13536, #15104, #12057, #108, #11962, #15193, #7356, #12151, #18057, #18156, #4714, #2958, #10679, #10390, #13720, #16682, #3248, #299, #13328, #3054, #17965, #4524, #12251, #19348, #18254, #9013, #4810, #5890, #11856, #17864, #4427, #16391, #5090, #9394, #6654, #483, #5176, #396, #15289, #4988, #6551, #12632, #9680, #15475, #3616, #9299, #1964, #2057, #16870, #12536, #15576, #10964, #6364, #15385, #7926, #13899, #682, #18636, #18549, #17064, #2155, #8018, #6453, #16973, #12434, #18442, #8117, #13992, #11147, #3525, #4900, #12341, #10863, #9488, #17155, #578, #11056, #9581, #14092, #3717, #3338, #1870, #7835, #13815, #18351, #3435, #16450, #4583, #9262, #16650, #10643, #5957, #15250, #3217, #18122, #7422, #3019, #16548, #9180, #1831, #4777, #13590, #12018, #18022, #8981, #10540, #3121 ),
 ( #1544, #13502, #13681, #13399, #18313, #77, #15159, #7612, #366, #13777, #7799, #1738, #6239, #6055, #6337, #9077, #4869, #10446, #18587, #165, #7702, #12309, #9357, #4685, #10739, #11923, #15070, #259, #7517, #12212, #3304, #6142, #14965, #1650, #12113, #18225, #10830, #16834, #16740, #3396, #1446, #17931, #4489, #641, #9549, #545, #11215, #3681, #12797, #6516, #9460, #10926, #2026, #17031, #5345, #3587, #5054, #15541, #12494, #15741, #14058, #15445, #3783, #11317, #18797, #2119, #16931, #18506, #9746, #11116, #5144, #451, #2320, #17123, #12596, #1934, #3496, #11025, #9647, #8273, #18697, #8082, #6618, #18605, #7986, #15642, #2224, #18410, #3878, #8183, #14155, #738, #6711, #15350, #12694, #5242, #17221, #14252, #836, #17321, #6809, #7898, #13959, #13870, #6423, #12403, #4953, #8479, #8576, #4168, #7097, #14543, #9937, #10226, #15837, #14638, #19091, #19195, #2622, #3973, #7199, #11409, #8764, #15937, #14742, #19290, #1127, #2421, #8373, #2803, #1328, #16038, #10133, #9836, #17414, #16135, #14458, #13082, #5632, #1040, #7003, #14353, #4261, #13274, #18897, #8666, #13181, #2714, #937, #12981, #11606, #5735, #2524, #5432, #17616, #7300, #18989, #5528, #11504, #5829, #17514, #4074, #6906, #1225, #11698, #10039, #17706, #16227, #11797, #12895, #17802, #13700, #9191, #8997, #4597, #10558, #13606, #4506, #1364, #2939, #8901, #14882, #4700, #3231, #16563, #15086, #185, #7533, #13416, #16467, #5974, #16373, #7627, #92, #15175, #1458, #5873, #7337, #17844, #3540, #1753 ),
 ( #11839, #6158, #7719, #276, #11943, #13314, #7437, #12131, #13518, #1563, #16271, #18138, #6072, #14980, #17744, #19331, #17947, #12039, #10660, #1664, #10463, #3034, #18037, #4404, #3137, #9098, #14785, #11739, #16667, #4303, #10268, #2846, #8812, #10373, #12417, #11039, #8003, #18526, #8202, #18620, #3414, #4884, #6349, #1848, #1948, #2041, #14076, #9566, #18427, #16853, #9374, #7815, #15366, #7910, #9279, #14171, #4969, #3510, #13882, #13974, #6253, #6532, #10944, #17045, #561, #5069, #12231, #5160, #466, #10847, #12325, #12516, #3601, #6634, #6438, #16951, #15558, #9473, #15459, #18331, #12613, #18239, #2138, #8098, #663, #11132, #381, #17140, #13795, #3701, #9662, #15659, #2248, #4794, #10757, #16754, #3321, #15269, #12711, #17634, #18815, #9953, #6927, #19109, #13100, #14561, #8500, #5546, #5361, #5649, #2438, #4183, #9769, #18714, #12909, #1053, #11622, #8686, #3990, #4090, #2730, #10150, #17431, #13004, #19009, #2639, #18913, #15762, #11334, #17342, #3897, #16151, #754, #11522, #10057, #8591, #15954, #8390, #5453, #14370, #9856, #16056, #14475, #6727, #15855, #14268, #2340, #6826, #954, #5261, #11428, #2541, #7022, #17530, #1146, #7119, #852, #11231, #17237, #3802, #8292, #12812, #17821, #3112, #10437, #4478, #19211, #9066, #16441, #11913, #1243, #15060, #3010, #69, #19307, #13580, #16345, #12104, #4278, #13197, #7412, #14955, #155, #3209, #17920, #18013, #16640, #18112, #8972, #7508, #13492, #16537, #13387, #10244, #5846, #11815, #4379, #7603, #6133, #6045, #4574 ) ),
 .UNSPECIFIED., .T., .F., .T. ) 
 B_SPLINE_SURFACE_WITH_KNOTS ( ( 4, 3, 4 ),
 ( 3, 2, 2, 2, 2, 2, 2, 2, 2, 2, 2, 2, 2, 2, 2, 2, 2, 2, 2, 2, 2, 2, 2, 2, 2, 2, 2, 2, 2, 2, 2, 2, 2, 2, 2, 2, 2, 2, 2, 2, 2, 2, 2, 2, 2, 2, 2, 2, 2, 2, 2, 2, 2, 2, 2, 2, 2, 2, 2, 2, 2, 2, 2, 2, 2, 2, 2, 2, 2, 2, 2, 2, 2, 2, 2, 2, 2, 2, 2, 2, 2, 2, 2, 2, 2, 2, 2, 2, 2, 2, 2, 2, 2, 2, 2, 2, 2, 2, 2, 2, 3 ),
 ( 0.000000000000000000, 0.5000000000000000000, 1.000000000000000000 ),
 ( 0.000000000000000000, 0.01000000000000000021, 0.02000000000000000042, 0.02999999999999999889, 0.04000000000000000083, 0.05000000000000000278, 0.05999999999999999778, 0.07000000000000000666, 0.08000000000000000167, 0.08999999999999999667, 0.1000000000000000056, 0.1100000000000000006, 0.1199999999999999956, 0.1300000000000000044, 0.1400000000000000133, 0.1499999999999999944, 0.1600000000000000033, 0.1700000000000000122, 0.1799999999999999933, 0.1900000000000000022, 0.2000000000000000111, 0.2099999999999999922, 0.2200000000000000011, 0.2300000000000000100, 0.2399999999999999911, 0.2500000000000000000, 0.2600000000000000089, 0.2700000000000000178, 0.2800000000000000266, 0.2899999999999999800, 0.2999999999999999889, 0.3099999999999999978, 0.3200000000000000067, 0.3300000000000000155, 0.3400000000000000244, 0.3499999999999999778, 0.3599999999999999867, 0.3699999999999999956, 0.3800000000000000044, 0.3900000000000000133, 0.4000000000000000222, 0.4099999999999999756, 0.4199999999999999845, 0.4299999999999999933, 0.4400000000000000022, 0.4500000000000000111, 0.4600000000000000200, 0.4699999999999999734, 0.4799999999999999822, 0.4899999999999999911, 0.5000000000000000000, 0.5100000000000000089, 0.5200000000000000178, 0.5300000000000000266, 0.5400000000000000355, 0.5500000000000000444, 0.5600000000000000533, 0.5699999999999999512, 0.5799999999999999600, 0.5899999999999999689, 0.5999999999999999778, 0.6099999999999999867, 0.6199999999999999956, 0.6300000000000000044, 0.6400000000000000133, 0.6500000000000000222, 0.6600000000000000311, 0.6700000000000000400, 0.6800000000000000488, 0.6899999999999999467, 0.6999999999999999556, 0.7099999999999999645, 0.7199999999999999734, 0.7299999999999999822, 0.7399999999999999911, 0.7500000000000000000, 0.7600000000000000089, 0.7700000000000000178, 0.7800000000000000266, 0.7900000000000000355, 0.8000000000000000444, 0.8100000000000000533, 0.8199999999999999512, 0.8299999999999999600, 0.8399999999999999689, 0.8499999999999999778, 0.8599999999999999867, 0.8699999999999999956, 0.8800000000000000044, 0.8900000000000000133, 0.9000000000000000222, 0.9100000000000000311, 0.9200000000000000400, 0.9300000000000000488, 0.9399999999999999467, 0.9499999999999999556, 0.9599999999999999645, 0.9699999999999999734, 0.9799999999999999822, 0.9899999999999999911, 1.000000000000000000 ),
 .UNSPECIFIED. ) 
 GEOMETRIC_REPRESENTATION_ITEM ( )  RATIONAL_B_SPLINE_SURFACE ( (
 ( 1.000000000000000000, 0.9510565162951535312, 1.000000000000000000, 0.9510565162951535312, 1.000000000000000000, 0.9510565162951535312, 1.000000000000000000, 0.9510565162951535312, 1.000000000000000000, 0.9510565162951535312, 1.000000000000000000, 0.9510565162951535312, 1.000000000000000000, 0.9510565162951535312, 1.000000000000000000, 0.9510565162951535312, 1.000000000000000000, 0.9510565162951535312, 1.000000000000000000, 0.9510565162951535312, 1.000000000000000000, 0.9510565162951535312, 1.000000000000000000, 0.9510565162951535312, 1.000000000000000000, 0.9510565162951535312, 1.000000000000000000, 0.9510565162951535312, 1.000000000000000000, 0.9510565162951535312, 1.000000000000000000, 0.9510565162951535312, 1.000000000000000000, 0.9510565162951535312, 1.000000000000000000, 0.9510565162951535312, 1.000000000000000000, 0.9510565162951535312, 1.000000000000000000, 0.9510565162951535312, 1.000000000000000000, 0.9510565162951535312, 1.000000000000000000, 0.9510565162951535312, 1.000000000000000000, 0.9510565162951535312, 1.000000000000000000, 0.9510565162951535312, 1.000000000000000000, 0.9510565162951535312, 1.000000000000000000, 0.9510565162951535312, 1.000000000000000000, 0.9510565162951535312, 1.000000000000000000, 0.9510565162951535312, 1.000000000000000000, 0.9510565162951535312, 1.000000000000000000, 0.9510565162951535312, 1.000000000000000000, 0.9510565162951535312, 1.000000000000000000, 0.9510565162951535312, 1.000000000000000000, 0.9510565162951535312, 1.000000000000000000, 0.9510565162951535312, 1.000000000000000000, 0.9510565162951535312, 1.000000000000000000, 0.9510565162951535312, 1.000000000000000000, 0.9510565162951535312, 1.000000000000000000, 0.9510565162951535312, 1.000000000000000000, 0.9510565162951535312, 1.000000000000000000, 0.9510565162951535312, 1.000000000000000000, 0.9510565162951535312, 1.000000000000000000, 0.9510565162951535312, 1.000000000000000000, 0.9510565162951535312, 1.000000000000000000, 0.9510565162951535312, 1.000000000000000000, 0.9510565162951535312, 1.000000000000000000, 0.9510565162951535312, 1.000000000000000000, 0.9510565162951535312, 1.000000000000000000, 0.9510565162951535312, 1.000000000000000000, 0.9510565162951535312, 1.000000000000000000, 0.9510565162951535312, 1.000000000000000000, 0.9510565162951535312, 1.000000000000000000, 0.9510565162951535312, 1.000000000000000000, 0.9510565162951535312, 1.000000000000000000, 0.9510565162951535312, 1.000000000000000000, 0.9510565162951535312, 1.000000000000000000, 0.9510565162951535312, 1.000000000000000000, 0.9510565162951535312, 1.000000000000000000, 0.9510565162951535312, 1.000000000000000000, 0.9510565162951535312, 1.000000000000000000, 0.9510565162951535312, 1.000000000000000000, 0.9510565162951535312, 1.000000000000000000, 0.9510565162951535312, 1.000000000000000000, 0.9510565162951535312, 1.000000000000000000, 0.9510565162951535312, 1.000000000000000000, 0.9510565162951535312, 1.000000000000000000, 0.9510565162951535312, 1.000000000000000000, 0.9510565162951535312, 1.000000000000000000, 0.9510565162951535312, 1.000000000000000000, 0.9510565162951535312, 1.000000000000000000, 0.9510565162951535312, 1.000000000000000000, 0.9510565162951535312, 1.000000000000000000, 0.9510565162951535312, 1.000000000000000000, 0.9510565162951535312, 1.000000000000000000, 0.9510565162951535312, 1.000000000000000000, 0.9510565162951535312, 1.000000000000000000, 0.9510565162951535312, 1.000000000000000000, 0.9510565162951535312, 1.000000000000000000, 0.9510565162951535312, 1.000000000000000000, 0.9510565162951535312, 1.000000000000000000, 0.9510565162951535312, 1.000000000000000000, 0.9510565162951535312, 1.000000000000000000, 0.9510565162951535312, 1.000000000000000000, 0.9510565162951535312, 1.000000000000000000, 0.9510565162951535312, 1.000000000000000000, 0.9510565162951535312, 1.000000000000000000, 0.9510565162951535312, 1.000000000000000000, 0.9510565162951535312, 1.000000000000000000, 0.9510565162951535312, 1.000000000000000000, 0.9510565162951535312, 1.000000000000000000, 0.9510565162951535312, 1.000000000000000000, 0.9510565162951535312, 1.000000000000000000, 0.9510565162951535312, 1.000000000000000000, 0.9510565162951535312, 1.000000000000000000, 0.9510565162951535312, 1.000000000000000000, 0.9510565162951535312, 1.000000000000000000, 0.9510565162951535312, 1.000000000000000000, 0.9510565162951535312, 1.000000000000000000, 0.9510565162951535312, 1.000000000000000000, 0.9510565162951535312, 1.000000000000000000, 0.9510565162951535312, 1.000000000000000000),
 ( 0.3333333333333333703, 0.3170188387650512141, 0.3333333333333333703, 0.3170188387650512141, 0.3333333333333333703, 0.3170188387650512141, 0.3333333333333333703, 0.3170188387650512141, 0.3333333333333333703, 0.3170188387650512141, 0.3333333333333333703, 0.3170188387650512141, 0.3333333333333333703, 0.3170188387650512141, 0.3333333333333333703, 0.3170188387650512141, 0.3333333333333333703, 0.3170188387650512141, 0.3333333333333333703, 0.3170188387650512141, 0.3333333333333333703, 0.3170188387650512141, 0.3333333333333333703, 0.3170188387650512141, 0.3333333333333333703, 0.3170188387650512141, 0.3333333333333333703, 0.3170188387650512141, 0.3333333333333333703, 0.3170188387650512141, 0.3333333333333333703, 0.3170188387650512141, 0.3333333333333333703, 0.3170188387650512141, 0.3333333333333333703, 0.3170188387650512141, 0.3333333333333333703, 0.3170188387650512141, 0.3333333333333333703, 0.3170188387650512141, 0.3333333333333333703, 0.3170188387650512141, 0.3333333333333333703, 0.3170188387650512141, 0.3333333333333333703, 0.3170188387650512141, 0.3333333333333333703, 0.3170188387650512141, 0.3333333333333333703, 0.3170188387650512141, 0.3333333333333333703, 0.3170188387650512141, 0.3333333333333333703, 0.3170188387650512141, 0.3333333333333333703, 0.3170188387650512141, 0.3333333333333333703, 0.3170188387650512141, 0.3333333333333333703, 0.3170188387650512141, 0.3333333333333333703, 0.3170188387650512141, 0.3333333333333333703, 0.3170188387650512141, 0.3333333333333333703, 0.3170188387650512141, 0.3333333333333333703, 0.3170188387650512141, 0.3333333333333333703, 0.3170188387650512141, 0.3333333333333333703, 0.3170188387650512141, 0.3333333333333333703, 0.3170188387650512141, 0.3333333333333333703, 0.3170188387650512141, 0.3333333333333333703, 0.3170188387650512141, 0.3333333333333333703, 0.3170188387650512141, 0.3333333333333333703, 0.3170188387650512141, 0.3333333333333333703, 0.3170188387650512141, 0.3333333333333333703, 0.3170188387650512141, 0.3333333333333333703, 0.3170188387650512141, 0.3333333333333333703, 0.3170188387650512141, 0.3333333333333333703, 0.3170188387650512141, 0.3333333333333333703, 0.3170188387650512141, 0.3333333333333333703, 0.3170188387650512141, 0.3333333333333333703, 0.3170188387650512141, 0.3333333333333333703, 0.3170188387650512141, 0.3333333333333333703, 0.3170188387650512141, 0.3333333333333333703, 0.3170188387650512141, 0.3333333333333333703, 0.3170188387650512141, 0.3333333333333333703, 0.3170188387650512141, 0.3333333333333333703, 0.3170188387650512141, 0.3333333333333333703, 0.3170188387650512141, 0.3333333333333333703, 0.3170188387650512141, 0.3333333333333333703, 0.3170188387650512141, 0.3333333333333333703, 0.3170188387650512141, 0.3333333333333333703, 0.3170188387650512141, 0.3333333333333333703, 0.3170188387650512141, 0.3333333333333333703, 0.3170188387650512141, 0.3333333333333333703, 0.3170188387650512141, 0.3333333333333333703, 0.3170188387650512141, 0.3333333333333333703, 0.3170188387650512141, 0.3333333333333333703, 0.3170188387650512141, 0.3333333333333333703, 0.3170188387650512141, 0.3333333333333333703, 0.3170188387650512141, 0.3333333333333333703, 0.3170188387650512141, 0.3333333333333333703, 0.3170188387650512141, 0.3333333333333333703, 0.3170188387650512141, 0.3333333333333333703, 0.3170188387650512141, 0.3333333333333333703, 0.3170188387650512141, 0.3333333333333333703, 0.3170188387650512141, 0.3333333333333333703, 0.3170188387650512141, 0.3333333333333333703, 0.3170188387650512141, 0.3333333333333333703, 0.3170188387650512141, 0.3333333333333333703, 0.3170188387650512141, 0.3333333333333333703, 0.3170188387650512141, 0.3333333333333333703, 0.3170188387650512141, 0.3333333333333333703, 0.3170188387650512141, 0.3333333333333333703, 0.3170188387650512141, 0.3333333333333333703, 0.3170188387650512141, 0.3333333333333333703, 0.3170188387650512141, 0.3333333333333333703, 0.3170188387650512141, 0.3333333333333333703, 0.3170188387650512141, 0.3333333333333333703, 0.3170188387650512141, 0.3333333333333333703, 0.3170188387650512141, 0.3333333333333333703, 0.3170188387650512141, 0.3333333333333333703, 0.3170188387650512141, 0.3333333333333333703, 0.3170188387650512141, 0.3333333333333333703, 0.3170188387650512141, 0.3333333333333333703, 0.3170188387650512141, 0.3333333333333333703, 0.3170188387650512141, 0.3333333333333333703, 0.3170188387650512141, 0.3333333333333333703, 0.3170188387650512141, 0.3333333333333333703, 0.3170188387650512141, 0.3333333333333333703, 0.3170188387650512141, 0.3333333333333333703, 0.3170188387650512141, 0.3333333333333333703, 0.3170188387650512141, 0.3333333333333333703),
 ( 0.3333333333333333703, 0.3170188387650512141, 0.3333333333333333703, 0.3170188387650512141, 0.3333333333333333703, 0.3170188387650512141, 0.3333333333333333703, 0.3170188387650512141, 0.3333333333333333703, 0.3170188387650512141, 0.3333333333333333703, 0.3170188387650512141, 0.3333333333333333703, 0.3170188387650512141, 0.3333333333333333703, 0.3170188387650512141, 0.3333333333333333703, 0.3170188387650512141, 0.3333333333333333703, 0.3170188387650512141, 0.3333333333333333703, 0.3170188387650512141, 0.3333333333333333703, 0.3170188387650512141, 0.3333333333333333703, 0.3170188387650512141, 0.3333333333333333703, 0.3170188387650512141, 0.3333333333333333703, 0.3170188387650512141, 0.3333333333333333703, 0.3170188387650512141, 0.3333333333333333703, 0.3170188387650512141, 0.3333333333333333703, 0.3170188387650512141, 0.3333333333333333703, 0.3170188387650512141, 0.3333333333333333703, 0.3170188387650512141, 0.3333333333333333703, 0.3170188387650512141, 0.3333333333333333703, 0.3170188387650512141, 0.3333333333333333703, 0.3170188387650512141, 0.3333333333333333703, 0.3170188387650512141, 0.3333333333333333703, 0.3170188387650512141, 0.3333333333333333703, 0.3170188387650512141, 0.3333333333333333703, 0.3170188387650512141, 0.3333333333333333703, 0.3170188387650512141, 0.3333333333333333703, 0.3170188387650512141, 0.3333333333333333703, 0.3170188387650512141, 0.3333333333333333703, 0.3170188387650512141, 0.3333333333333333703, 0.3170188387650512141, 0.3333333333333333703, 0.3170188387650512141, 0.3333333333333333703, 0.3170188387650512141, 0.3333333333333333703, 0.3170188387650512141, 0.3333333333333333703, 0.3170188387650512141, 0.3333333333333333703, 0.3170188387650512141, 0.3333333333333333703, 0.3170188387650512141, 0.3333333333333333703, 0.3170188387650512141, 0.3333333333333333703, 0.3170188387650512141, 0.3333333333333333703, 0.3170188387650512141, 0.3333333333333333703, 0.3170188387650512141, 0.3333333333333333703, 0.3170188387650512141, 0.3333333333333333703, 0.3170188387650512141, 0.3333333333333333703, 0.3170188387650512141, 0.3333333333333333703, 0.3170188387650512141, 0.3333333333333333703, 0.3170188387650512141, 0.3333333333333333703, 0.3170188387650512141, 0.3333333333333333703, 0.3170188387650512141, 0.3333333333333333703, 0.3170188387650512141, 0.3333333333333333703, 0.3170188387650512141, 0.3333333333333333703, 0.3170188387650512141, 0.3333333333333333703, 0.3170188387650512141, 0.3333333333333333703, 0.3170188387650512141, 0.3333333333333333703, 0.3170188387650512141, 0.3333333333333333703, 0.3170188387650512141, 0.3333333333333333703, 0.3170188387650512141, 0.3333333333333333703, 0.3170188387650512141, 0.3333333333333333703, 0.3170188387650512141, 0.3333333333333333703, 0.3170188387650512141, 0.3333333333333333703, 0.3170188387650512141, 0.3333333333333333703, 0.3170188387650512141, 0.3333333333333333703, 0.3170188387650512141, 0.3333333333333333703, 0.3170188387650512141, 0.3333333333333333703, 0.3170188387650512141, 0.3333333333333333703, 0.3170188387650512141, 0.3333333333333333703, 0.3170188387650512141, 0.3333333333333333703, 0.3170188387650512141, 0.3333333333333333703, 0.3170188387650512141, 0.3333333333333333703, 0.3170188387650512141, 0.3333333333333333703, 0.3170188387650512141, 0.3333333333333333703, 0.3170188387650512141, 0.3333333333333333703, 0.3170188387650512141, 0.3333333333333333703, 0.3170188387650512141, 0.3333333333333333703, 0.3170188387650512141, 0.3333333333333333703, 0.3170188387650512141, 0.3333333333333333703, 0.3170188387650512141, 0.3333333333333333703, 0.3170188387650512141, 0.3333333333333333703, 0.3170188387650512141, 0.3333333333333333703, 0.3170188387650512141, 0.3333333333333333703, 0.3170188387650512141, 0.3333333333333333703, 0.3170188387650512141, 0.3333333333333333703, 0.3170188387650512141, 0.3333333333333333703, 0.3170188387650512141, 0.3333333333333333703, 0.3170188387650512141, 0.3333333333333333703, 0.3170188387650512141, 0.3333333333333333703, 0.3170188387650512141, 0.3333333333333333703, 0.3170188387650512141, 0.3333333333333333703, 0.3170188387650512141, 0.3333333333333333703, 0.3170188387650512141, 0.3333333333333333703, 0.3170188387650512141, 0.3333333333333333703, 0.3170188387650512141, 0.3333333333333333703, 0.3170188387650512141, 0.3333333333333333703, 0.3170188387650512141, 0.3333333333333333703, 0.3170188387650512141, 0.3333333333333333703, 0.3170188387650512141, 0.3333333333333333703, 0.3170188387650512141, 0.3333333333333333703, 0.3170188387650512141, 0.3333333333333333703, 0.3170188387650512141, 0.3333333333333333703, 0.3170188387650512141, 0.3333333333333333703),
 ( 1.000000000000000000, 0.9510565162951535312, 1.000000000000000000, 0.9510565162951535312, 1.000000000000000000, 0.9510565162951535312, 1.000000000000000000, 0.9510565162951535312, 1.000000000000000000, 0.9510565162951535312, 1.000000000000000000, 0.9510565162951535312, 1.000000000000000000, 0.9510565162951535312, 1.000000000000000000, 0.9510565162951535312, 1.000000000000000000, 0.9510565162951535312, 1.000000000000000000, 0.9510565162951535312, 1.000000000000000000, 0.9510565162951535312, 1.000000000000000000, 0.9510565162951535312, 1.000000000000000000, 0.9510565162951535312, 1.000000000000000000, 0.9510565162951535312, 1.000000000000000000, 0.9510565162951535312, 1.000000000000000000, 0.9510565162951535312, 1.000000000000000000, 0.9510565162951535312, 1.000000000000000000, 0.9510565162951535312, 1.000000000000000000, 0.9510565162951535312, 1.000000000000000000, 0.9510565162951535312, 1.000000000000000000, 0.9510565162951535312, 1.000000000000000000, 0.9510565162951535312, 1.000000000000000000, 0.9510565162951535312, 1.000000000000000000, 0.9510565162951535312, 1.000000000000000000, 0.9510565162951535312, 1.000000000000000000, 0.9510565162951535312, 1.000000000000000000, 0.9510565162951535312, 1.000000000000000000, 0.9510565162951535312, 1.000000000000000000, 0.9510565162951535312, 1.000000000000000000, 0.9510565162951535312, 1.000000000000000000, 0.9510565162951535312, 1.000000000000000000, 0.9510565162951535312, 1.000000000000000000, 0.9510565162951535312, 1.000000000000000000, 0.9510565162951535312, 1.000000000000000000, 0.9510565162951535312, 1.000000000000000000, 0.9510565162951535312, 1.000000000000000000, 0.9510565162951535312, 1.000000000000000000, 0.9510565162951535312, 1.000000000000000000, 0.9510565162951535312, 1.000000000000000000, 0.9510565162951535312, 1.000000000000000000, 0.9510565162951535312, 1.000000000000000000, 0.9510565162951535312, 1.000000000000000000, 0.9510565162951535312, 1.000000000000000000, 0.9510565162951535312, 1.000000000000000000, 0.9510565162951535312, 1.000000000000000000, 0.9510565162951535312, 1.000000000000000000, 0.9510565162951535312, 1.000000000000000000, 0.9510565162951535312, 1.000000000000000000, 0.9510565162951535312, 1.000000000000000000, 0.9510565162951535312, 1.000000000000000000, 0.9510565162951535312, 1.000000000000000000, 0.9510565162951535312, 1.000000000000000000, 0.9510565162951535312, 1.000000000000000000, 0.9510565162951535312, 1.000000000000000000, 0.9510565162951535312, 1.000000000000000000, 0.9510565162951535312, 1.000000000000000000, 0.9510565162951535312, 1.000000000000000000, 0.9510565162951535312, 1.000000000000000000, 0.9510565162951535312, 1.000000000000000000, 0.9510565162951535312, 1.000000000000000000, 0.9510565162951535312, 1.000000000000000000, 0.9510565162951535312, 1.000000000000000000, 0.9510565162951535312, 1.000000000000000000, 0.9510565162951535312, 1.000000000000000000, 0.9510565162951535312, 1.000000000000000000, 0.9510565162951535312, 1.000000000000000000, 0.9510565162951535312, 1.000000000000000000, 0.9510565162951535312, 1.000000000000000000, 0.9510565162951535312, 1.000000000000000000, 0.9510565162951535312, 1.000000000000000000, 0.9510565162951535312, 1.000000000000000000, 0.9510565162951535312, 1.000000000000000000, 0.9510565162951535312, 1.000000000000000000, 0.9510565162951535312, 1.000000000000000000, 0.9510565162951535312, 1.000000000000000000, 0.9510565162951535312, 1.000000000000000000, 0.9510565162951535312, 1.000000000000000000, 0.9510565162951535312, 1.000000000000000000, 0.9510565162951535312, 1.000000000000000000, 0.9510565162951535312, 1.000000000000000000, 0.9510565162951535312, 1.000000000000000000, 0.9510565162951535312, 1.000000000000000000, 0.9510565162951535312, 1.000000000000000000, 0.9510565162951535312, 1.000000000000000000, 0.9510565162951535312, 1.000000000000000000, 0.9510565162951535312, 1.000000000000000000, 0.9510565162951535312, 1.000000000000000000, 0.9510565162951535312, 1.000000000000000000, 0.9510565162951535312, 1.000000000000000000, 0.9510565162951535312, 1.000000000000000000, 0.9510565162951535312, 1.000000000000000000, 0.9510565162951535312, 1.000000000000000000, 0.9510565162951535312, 1.000000000000000000, 0.9510565162951535312, 1.000000000000000000, 0.9510565162951535312, 1.000000000000000000, 0.9510565162951535312, 1.000000000000000000, 0.9510565162951535312, 1.000000000000000000, 0.9510565162951535312, 1.000000000000000000, 0.9510565162951535312, 1.000000000000000000, 0.9510565162951535312, 1.000000000000000000),
 ( 0.3333333333333333703, 0.3170188387650512141, 0.3333333333333333703, 0.3170188387650512141, 0.3333333333333333703, 0.3170188387650512141, 0.3333333333333333703, 0.3170188387650512141, 0.3333333333333333703, 0.3170188387650512141, 0.3333333333333333703, 0.3170188387650512141, 0.3333333333333333703, 0.3170188387650512141, 0.3333333333333333703, 0.3170188387650512141, 0.3333333333333333703, 0.3170188387650512141, 0.3333333333333333703, 0.3170188387650512141, 0.3333333333333333703, 0.3170188387650512141, 0.3333333333333333703, 0.3170188387650512141, 0.3333333333333333703, 0.3170188387650512141, 0.3333333333333333703, 0.3170188387650512141, 0.3333333333333333703, 0.3170188387650512141, 0.3333333333333333703, 0.3170188387650512141, 0.3333333333333333703, 0.3170188387650512141, 0.3333333333333333703, 0.3170188387650512141, 0.3333333333333333703, 0.3170188387650512141, 0.3333333333333333703, 0.3170188387650512141, 0.3333333333333333703, 0.3170188387650512141, 0.3333333333333333703, 0.3170188387650512141, 0.3333333333333333703, 0.3170188387650512141, 0.3333333333333333703, 0.3170188387650512141, 0.3333333333333333703, 0.3170188387650512141, 0.3333333333333333703, 0.3170188387650512141, 0.3333333333333333703, 0.3170188387650512141, 0.3333333333333333703, 0.3170188387650512141, 0.3333333333333333703, 0.3170188387650512141, 0.3333333333333333703, 0.3170188387650512141, 0.3333333333333333703, 0.3170188387650512141, 0.3333333333333333703, 0.3170188387650512141, 0.3333333333333333703, 0.3170188387650512141, 0.3333333333333333703, 0.3170188387650512141, 0.3333333333333333703, 0.3170188387650512141, 0.3333333333333333703, 0.3170188387650512141, 0.3333333333333333703, 0.3170188387650512141, 0.3333333333333333703, 0.3170188387650512141, 0.3333333333333333703, 0.3170188387650512141, 0.3333333333333333703, 0.3170188387650512141, 0.3333333333333333703, 0.3170188387650512141, 0.3333333333333333703, 0.3170188387650512141, 0.3333333333333333703, 0.3170188387650512141, 0.3333333333333333703, 0.3170188387650512141, 0.3333333333333333703, 0.3170188387650512141, 0.3333333333333333703, 0.3170188387650512141, 0.3333333333333333703, 0.3170188387650512141, 0.3333333333333333703, 0.3170188387650512141, 0.3333333333333333703, 0.3170188387650512141, 0.3333333333333333703, 0.3170188387650512141, 0.3333333333333333703, 0.3170188387650512141, 0.3333333333333333703, 0.3170188387650512141, 0.3333333333333333703, 0.3170188387650512141, 0.3333333333333333703, 0.3170188387650512141, 0.3333333333333333703, 0.3170188387650512141, 0.3333333333333333703, 0.3170188387650512141, 0.3333333333333333703, 0.3170188387650512141, 0.3333333333333333703, 0.3170188387650512141, 0.3333333333333333703, 0.3170188387650512141, 0.3333333333333333703, 0.3170188387650512141, 0.3333333333333333703, 0.3170188387650512141, 0.3333333333333333703, 0.3170188387650512141, 0.3333333333333333703, 0.3170188387650512141, 0.3333333333333333703, 0.3170188387650512141, 0.3333333333333333703, 0.3170188387650512141, 0.3333333333333333703, 0.3170188387650512141, 0.3333333333333333703, 0.3170188387650512141, 0.3333333333333333703, 0.3170188387650512141, 0.3333333333333333703, 0.3170188387650512141, 0.3333333333333333703, 0.3170188387650512141, 0.3333333333333333703, 0.3170188387650512141, 0.3333333333333333703, 0.3170188387650512141, 0.3333333333333333703, 0.3170188387650512141, 0.3333333333333333703, 0.3170188387650512141, 0.3333333333333333703, 0.3170188387650512141, 0.3333333333333333703, 0.3170188387650512141, 0.3333333333333333703, 0.3170188387650512141, 0.3333333333333333703, 0.3170188387650512141, 0.3333333333333333703, 0.3170188387650512141, 0.3333333333333333703, 0.3170188387650512141, 0.3333333333333333703, 0.3170188387650512141, 0.3333333333333333703, 0.3170188387650512141, 0.3333333333333333703, 0.3170188387650512141, 0.3333333333333333703, 0.3170188387650512141, 0.3333333333333333703, 0.3170188387650512141, 0.3333333333333333703, 0.3170188387650512141, 0.3333333333333333703, 0.3170188387650512141, 0.3333333333333333703, 0.3170188387650512141, 0.3333333333333333703, 0.3170188387650512141, 0.3333333333333333703, 0.3170188387650512141, 0.3333333333333333703, 0.3170188387650512141, 0.3333333333333333703, 0.3170188387650512141, 0.3333333333333333703, 0.3170188387650512141, 0.3333333333333333703, 0.3170188387650512141, 0.3333333333333333703, 0.3170188387650512141, 0.3333333333333333703, 0.3170188387650512141, 0.3333333333333333703, 0.3170188387650512141, 0.3333333333333333703, 0.3170188387650512141, 0.3333333333333333703, 0.3170188387650512141, 0.3333333333333333703, 0.3170188387650512141, 0.3333333333333333703),
 ( 0.3333333333333333703, 0.3170188387650512141, 0.3333333333333333703, 0.3170188387650512141, 0.3333333333333333703, 0.3170188387650512141, 0.3333333333333333703, 0.3170188387650512141, 0.3333333333333333703, 0.3170188387650512141, 0.3333333333333333703, 0.3170188387650512141, 0.3333333333333333703, 0.3170188387650512141, 0.3333333333333333703, 0.3170188387650512141, 0.3333333333333333703, 0.3170188387650512141, 0.3333333333333333703, 0.3170188387650512141, 0.3333333333333333703, 0.3170188387650512141, 0.3333333333333333703, 0.3170188387650512141, 0.3333333333333333703, 0.3170188387650512141, 0.3333333333333333703, 0.3170188387650512141, 0.3333333333333333703, 0.3170188387650512141, 0.3333333333333333703, 0.3170188387650512141, 0.3333333333333333703, 0.3170188387650512141, 0.3333333333333333703, 0.3170188387650512141, 0.3333333333333333703, 0.3170188387650512141, 0.3333333333333333703, 0.3170188387650512141, 0.3333333333333333703, 0.3170188387650512141, 0.3333333333333333703, 0.3170188387650512141, 0.3333333333333333703, 0.3170188387650512141, 0.3333333333333333703, 0.3170188387650512141, 0.3333333333333333703, 0.3170188387650512141, 0.3333333333333333703, 0.3170188387650512141, 0.3333333333333333703, 0.3170188387650512141, 0.3333333333333333703, 0.3170188387650512141, 0.3333333333333333703, 0.3170188387650512141, 0.3333333333333333703, 0.3170188387650512141, 0.3333333333333333703, 0.3170188387650512141, 0.3333333333333333703, 0.3170188387650512141, 0.3333333333333333703, 0.3170188387650512141, 0.3333333333333333703, 0.3170188387650512141, 0.3333333333333333703, 0.3170188387650512141, 0.3333333333333333703, 0.3170188387650512141, 0.3333333333333333703, 0.3170188387650512141, 0.3333333333333333703, 0.3170188387650512141, 0.3333333333333333703, 0.3170188387650512141, 0.3333333333333333703, 0.3170188387650512141, 0.3333333333333333703, 0.3170188387650512141, 0.3333333333333333703, 0.3170188387650512141, 0.3333333333333333703, 0.3170188387650512141, 0.3333333333333333703, 0.3170188387650512141, 0.3333333333333333703, 0.3170188387650512141, 0.3333333333333333703, 0.3170188387650512141, 0.3333333333333333703, 0.3170188387650512141, 0.3333333333333333703, 0.3170188387650512141, 0.3333333333333333703, 0.3170188387650512141, 0.3333333333333333703, 0.3170188387650512141, 0.3333333333333333703, 0.3170188387650512141, 0.3333333333333333703, 0.3170188387650512141, 0.3333333333333333703, 0.3170188387650512141, 0.3333333333333333703, 0.3170188387650512141, 0.3333333333333333703, 0.3170188387650512141, 0.3333333333333333703, 0.3170188387650512141, 0.3333333333333333703, 0.3170188387650512141, 0.3333333333333333703, 0.3170188387650512141, 0.3333333333333333703, 0.3170188387650512141, 0.3333333333333333703, 0.3170188387650512141, 0.3333333333333333703, 0.3170188387650512141, 0.3333333333333333703, 0.3170188387650512141, 0.3333333333333333703, 0.3170188387650512141, 0.3333333333333333703, 0.3170188387650512141, 0.3333333333333333703, 0.3170188387650512141, 0.3333333333333333703, 0.3170188387650512141, 0.3333333333333333703, 0.3170188387650512141, 0.3333333333333333703, 0.3170188387650512141, 0.3333333333333333703, 0.3170188387650512141, 0.3333333333333333703, 0.3170188387650512141, 0.3333333333333333703, 0.3170188387650512141, 0.3333333333333333703, 0.3170188387650512141, 0.3333333333333333703, 0.3170188387650512141, 0.3333333333333333703, 0.3170188387650512141, 0.3333333333333333703, 0.3170188387650512141, 0.3333333333333333703, 0.3170188387650512141, 0.3333333333333333703, 0.3170188387650512141, 0.3333333333333333703, 0.3170188387650512141, 0.3333333333333333703, 0.3170188387650512141, 0.3333333333333333703, 0.3170188387650512141, 0.3333333333333333703, 0.3170188387650512141, 0.3333333333333333703, 0.3170188387650512141, 0.3333333333333333703, 0.3170188387650512141, 0.3333333333333333703, 0.3170188387650512141, 0.3333333333333333703, 0.3170188387650512141, 0.3333333333333333703, 0.3170188387650512141, 0.3333333333333333703, 0.3170188387650512141, 0.3333333333333333703, 0.3170188387650512141, 0.3333333333333333703, 0.3170188387650512141, 0.3333333333333333703, 0.3170188387650512141, 0.3333333333333333703, 0.3170188387650512141, 0.3333333333333333703, 0.3170188387650512141, 0.3333333333333333703, 0.3170188387650512141, 0.3333333333333333703, 0.3170188387650512141, 0.3333333333333333703, 0.3170188387650512141, 0.3333333333333333703, 0.3170188387650512141, 0.3333333333333333703, 0.3170188387650512141, 0.3333333333333333703, 0.3170188387650512141, 0.3333333333333333703, 0.3170188387650512141, 0.3333333333333333703, 0.3170188387650512141, 0.3333333333333333703),
 ( 1.000000000000000000, 0.9510565162951535312, 1.000000000000000000, 0.9510565162951535312, 1.000000000000000000, 0.9510565162951535312, 1.000000000000000000, 0.9510565162951535312, 1.000000000000000000, 0.9510565162951535312, 1.000000000000000000, 0.9510565162951535312, 1.000000000000000000, 0.9510565162951535312, 1.000000000000000000, 0.9510565162951535312, 1.000000000000000000, 0.9510565162951535312, 1.000000000000000000, 0.9510565162951535312, 1.000000000000000000, 0.9510565162951535312, 1.000000000000000000, 0.9510565162951535312, 1.000000000000000000, 0.9510565162951535312, 1.000000000000000000, 0.9510565162951535312, 1.000000000000000000, 0.9510565162951535312, 1.000000000000000000, 0.9510565162951535312, 1.000000000000000000, 0.9510565162951535312, 1.000000000000000000, 0.9510565162951535312, 1.000000000000000000, 0.9510565162951535312, 1.000000000000000000, 0.9510565162951535312, 1.000000000000000000, 0.9510565162951535312, 1.000000000000000000, 0.9510565162951535312, 1.000000000000000000, 0.9510565162951535312, 1.000000000000000000, 0.9510565162951535312, 1.000000000000000000, 0.9510565162951535312, 1.000000000000000000, 0.9510565162951535312, 1.000000000000000000, 0.9510565162951535312, 1.000000000000000000, 0.9510565162951535312, 1.000000000000000000, 0.9510565162951535312, 1.000000000000000000, 0.9510565162951535312, 1.000000000000000000, 0.9510565162951535312, 1.000000000000000000, 0.9510565162951535312, 1.000000000000000000, 0.9510565162951535312, 1.000000000000000000, 0.9510565162951535312, 1.000000000000000000, 0.9510565162951535312, 1.000000000000000000, 0.9510565162951535312, 1.000000000000000000, 0.9510565162951535312, 1.000000000000000000, 0.9510565162951535312, 1.000000000000000000, 0.9510565162951535312, 1.000000000000000000, 0.9510565162951535312, 1.000000000000000000, 0.9510565162951535312, 1.000000000000000000, 0.9510565162951535312, 1.000000000000000000, 0.9510565162951535312, 1.000000000000000000, 0.9510565162951535312, 1.000000000000000000, 0.9510565162951535312, 1.000000000000000000, 0.9510565162951535312, 1.000000000000000000, 0.9510565162951535312, 1.000000000000000000, 0.9510565162951535312, 1.000000000000000000, 0.9510565162951535312, 1.000000000000000000, 0.9510565162951535312, 1.000000000000000000, 0.9510565162951535312, 1.000000000000000000, 0.9510565162951535312, 1.000000000000000000, 0.9510565162951535312, 1.000000000000000000, 0.9510565162951535312, 1.000000000000000000, 0.9510565162951535312, 1.000000000000000000, 0.9510565162951535312, 1.000000000000000000, 0.9510565162951535312, 1.000000000000000000, 0.9510565162951535312, 1.000000000000000000, 0.9510565162951535312, 1.000000000000000000, 0.9510565162951535312, 1.000000000000000000, 0.9510565162951535312, 1.000000000000000000, 0.9510565162951535312, 1.000000000000000000, 0.9510565162951535312, 1.000000000000000000, 0.9510565162951535312, 1.000000000000000000, 0.9510565162951535312, 1.000000000000000000, 0.9510565162951535312, 1.000000000000000000, 0.9510565162951535312, 1.000000000000000000, 0.9510565162951535312, 1.000000000000000000, 0.9510565162951535312, 1.000000000000000000, 0.9510565162951535312, 1.000000000000000000, 0.9510565162951535312, 1.000000000000000000, 0.9510565162951535312, 1.000000000000000000, 0.9510565162951535312, 1.000000000000000000, 0.9510565162951535312, 1.000000000000000000, 0.9510565162951535312, 1.000000000000000000, 0.9510565162951535312, 1.000000000000000000, 0.9510565162951535312, 1.000000000000000000, 0.9510565162951535312, 1.000000000000000000, 0.9510565162951535312, 1.000000000000000000, 0.9510565162951535312, 1.000000000000000000, 0.9510565162951535312, 1.000000000000000000, 0.9510565162951535312, 1.000000000000000000, 0.9510565162951535312, 1.000000000000000000, 0.9510565162951535312, 1.000000000000000000, 0.9510565162951535312, 1.000000000000000000, 0.9510565162951535312, 1.000000000000000000, 0.9510565162951535312, 1.000000000000000000, 0.9510565162951535312, 1.000000000000000000, 0.9510565162951535312, 1.000000000000000000, 0.9510565162951535312, 1.000000000000000000, 0.9510565162951535312, 1.000000000000000000, 0.9510565162951535312, 1.000000000000000000, 0.9510565162951535312, 1.000000000000000000, 0.9510565162951535312, 1.000000000000000000, 0.9510565162951535312, 1.000000000000000000, 0.9510565162951535312, 1.000000000000000000, 0.9510565162951535312, 1.000000000000000000, 0.9510565162951535312, 1.000000000000000000, 0.9510565162951535312, 1.000000000000000000, 0.9510565162951535312, 1.000000000000000000) ) ) 
 REPRESENTATION_ITEM ( '' )  SURFACE ( )  );
#14558 = ORIENTED_EDGE ( 'NONE', *, *, #18402, .F. ) ;
#14559 = LINE ( 'NONE', #11711, #18467 ) ;
#14560 = VERTEX_POINT ( 'NONE', #5917 ) ;
#14561 = CARTESIAN_POINT ( 'NONE',  ( 57.36023556966787851, 55.99948385550239038, -0.02388180880522424582 ) ) ;
#14562 = DIRECTION ( 'NONE',  ( -1.000000000000000000, 0.000000000000000000, 0.000000000000000000 ) ) ;
#14563 = ORIENTED_EDGE ( 'NONE', *, *, #9969, .F. ) ;
#14564 = VERTEX_POINT ( 'NONE', #17695 ) ;
#14565 = CARTESIAN_POINT ( 'NONE',  ( 2.000000000000000000, -0.8865213383406694847, 1.535500000000001419 ) ) ;
#14566 = AXIS2_PLACEMENT_3D ( 'NONE', #115, #17974, #10491 ) ;
#14567 = DIRECTION ( 'NONE',  ( -1.000000000000000000, 0.000000000000000000, 0.000000000000000000 ) ) ;
#14568 = VERTEX_POINT ( 'NONE', #19280 ) ;
#14569 = CARTESIAN_POINT ( 'NONE',  ( 0.01055556052338981095, 4.575665857285978078, 2.074714256722482997 ) ) ;
#14570 = ORIENTED_EDGE ( 'NONE', *, *, #5301, .F. ) ;
#14571 = CARTESIAN_POINT ( 'NONE',  ( 0.1750025118121568690, 4.719839900820621104, -3.469254087858248070 ) ) ;
#14572 = CARTESIAN_POINT ( 'NONE',  ( 54.09612160359786515, 51.69948385550240744, -5.676469297603166098 ) ) ;
#14573 = PRESENTATION_LAYER_ASSIGNMENT (  '', '', ( #10189 ) ) ;
#14574 = DIRECTION ( 'NONE',  ( -1.000000000000000000, 0.000000000000000000, 0.000000000000000000 ) ) ;
#14575 = CARTESIAN_POINT ( 'NONE',  ( 43.34962307344078880, 50.10051614449766078, -2.184720259617096705 ) ) ;
#14576 = CARTESIAN_POINT ( 'NONE',  ( 53.50000000000000000, 0.000000000000000000, 3.309499999999999886 ) ) ;
#14577 = DIRECTION ( 'NONE',  ( 0.000000000000000000, 0.000000000000000000, 1.000000000000000000 ) ) ;
#14578 = EDGE_CURVE ( 'NONE', #11631, #7961, #911, .T. ) ;
#14579 = DIRECTION ( 'NONE',  ( 1.000000000000000000, 0.000000000000000000, 0.000000000000000000 ) ) ;
#14580 = VECTOR ( 'NONE', #10849, 1000.000000000000000 ) ;
#14581 = ADVANCED_FACE ( 'NONE', ( #10124 ), #4347, .F. ) ;
#14582 = ORIENTED_EDGE ( 'NONE', *, *, #16258, .T. ) ;
#14583 = ORIENTED_EDGE ( 'NONE', *, *, #5209, .F. ) ;
#14584 = CARTESIAN_POINT ( 'NONE',  ( 2.449293598294706513E-15, -20.00000000000000000, 9.000000000000000000 ) ) ;
#14585 = DIRECTION ( 'NONE',  ( -1.000000000000000000, 0.000000000000000000, -0.000000000000000000 ) ) ;
#14586 = CIRCLE ( 'NONE', #9267, 7.000000000000000000 ) ;
#14587 = DIRECTION ( 'NONE',  ( 0.000000000000000000, -0.000000000000000000, 1.000000000000000000 ) ) ;
#14588 = ORIENTED_EDGE ( 'NONE', *, *, #5704, .T. ) ;
#14589 = CARTESIAN_POINT ( 'NONE',  ( -19.02113032590308705, -13.81966011250110249, 9.000000000000000000 ) ) ;
#14590 = ORIENTED_EDGE ( 'NONE', *, *, #5545, .F. ) ;
#14591 = VERTEX_POINT ( 'NONE', #13264 ) ;
#14592 = EDGE_CURVE ( 'NONE', #9732, #4952, #4374, .T. ) ;
#14593 = CARTESIAN_POINT ( 'NONE',  ( 4.799999999999999822, 0.000000000000000000, 0.000000000000000000 ) ) ;
#14594 = FACE_OUTER_BOUND ( 'NONE', #2106, .T. ) ;
#14595 = CARTESIAN_POINT ( 'NONE',  ( 48.02776887271750184, 49.60051614449766788, 5.992620115222795363 ) ) ;
#14596 = CARTESIAN_POINT ( 'NONE',  ( 75.00000000000001421, -39.99999999999998579, -10.00000000000000000 ) ) ;
#14597 = ADVANCED_FACE ( 'NONE', ( #5818 ), #2793, .T. ) ;
#14598 = DIRECTION ( 'NONE',  ( 0.000000000000000000, 0.000000000000000000, 1.000000000000000000 ) ) ;
#14599 = CARTESIAN_POINT ( 'NONE',  ( 55.71335778527780747, 54.09948385550241312, 1.832500667257165983 ) ) ;
#14600 = LINE ( 'NONE', #1090, #9083 ) ;
#14601 = CARTESIAN_POINT ( 'NONE',  ( 56.81924384183011512, 64.19948385550240744, 4.924951120819313743 ) ) ;
#14602 = CARTESIAN_POINT ( 'NONE',  ( 42.38452918213190657, 47.90051614449765793, 2.450534656007115508 ) ) ;
#14603 = CARTESIAN_POINT ( 'NONE',  ( 0.000000000000000000, 0.8865213383406680414, -1.535500000000000975 ) ) ;
#14604 = CARTESIAN_POINT ( 'NONE',  ( 2.449293598294706513E-15, -20.00000000000000000, -9.000000000000000000 ) ) ;
#14605 = CIRCLE ( 'NONE', #8659, 0.1000000000000002554 ) ;
#14606 = PRODUCT_CONTEXT ( 'NONE', #10873, 'mechanical' ) ;
#14607 = ORIENTED_EDGE ( 'NONE', *, *, #11609, .F. ) ;
#14608 = CARTESIAN_POINT ( 'NONE',  ( -1.274258131565027874, -3.883108878240886241, -3.220599429844051009 ) ) ;
#14609 = VECTOR ( 'NONE', #16989, 1000.000000000000000 ) ;
#14610 = PRODUCT_DEFINITION_SHAPE ( 'NONE', 'NONE',  #19434 ) ;
#14611 = DIRECTION ( 'NONE',  ( 0.000000000000000000, 0.000000000000000000, -1.000000000000000000 ) ) ;
#14612 = VECTOR ( 'NONE', #9235, 1000.000000000000000 ) ;
#14613 = CARTESIAN_POINT ( 'NONE',  ( 1.411581201560190495E-15, 4.862606272033091592, -3.745885042887436622 ) ) ;
#14614 = DIRECTION ( 'NONE',  ( -1.000000000000000000, 0.000000000000000000, 0.000000000000000000 ) ) ;
#14615 = ORIENTED_EDGE ( 'NONE', *, *, #19061, .F. ) ;
#14616 = CIRCLE ( 'NONE', #8037, 4.000000000000031086 ) ;
#14617 = DIRECTION ( 'NONE',  ( -1.000000000000000000, -0.000000000000000000, -0.000000000000000000 ) ) ;
#14618 = DIRECTION ( 'NONE',  ( 1.000000000000000000, 0.000000000000000000, 0.000000000000000000 ) ) ;
#14619 = CARTESIAN_POINT ( 'NONE',  ( 43.34962307344081012, 54.89948385550240317, 2.184720259617164650 ) ) ;
#14620 = CARTESIAN_POINT ( 'NONE',  ( 1.000000000000000000, -5.408326913195983465, -0.8000000000000000444 ) ) ;
#14621 = CARTESIAN_POINT ( 'NONE',  ( 54.68390685589033495, 49.69948385550240744, -6.485486291978119766 ) ) ;
#14622 = CARTESIAN_POINT ( 'NONE',  ( 49.97728705011495265, 45.50051614449765935, 7.000000000000000888 ) ) ;
#14623 = AXIS2_PLACEMENT_3D ( 'NONE', #17081, #16991, #13734 ) ;
#14624 = CARTESIAN_POINT ( 'NONE',  ( -150.9999999999999432, -14.99999999999999645, 17.00000000000000000 ) ) ;
#14625 = ORIENTED_EDGE ( 'NONE', *, *, #15134, .F. ) ;
#14626 = EDGE_LOOP ( 'NONE', ( #8599, #2641, #8173, #12906 ) ) ;
#14627 = CYLINDRICAL_SURFACE ( 'NONE', #4980, 4.000000000000031086 ) ;
#14628 = PRESENTATION_LAYER_ASSIGNMENT (  '', '', ( #3073 ) ) ;
#14629 = ORIENTED_EDGE ( 'NONE', *, *, #8957, .F. ) ;
#14630 = FACE_OUTER_BOUND ( 'NONE', #3896, .T. ) ;
#14631 = EDGE_LOOP ( 'NONE', ( #9327, #3515, #15530, #14225, #15275, #8616, #18784, #5981, #19232, #11311, #9708, #6605 ) ) ;
#14632 = DIRECTION ( 'NONE',  ( 0.000000000000000000, 0.000000000000000000, 1.000000000000000000 ) ) ;
#14633 = EDGE_CURVE ( 'NONE', #19111, #10629, #16895, .T. ) ;
#14634 = VERTEX_POINT ( 'NONE', #3252 ) ;
#14635 = DIRECTION ( 'NONE',  ( 0.000000000000000000, 0.000000000000000000, -1.000000000000000000 ) ) ;
#14636 = ORIENTED_EDGE ( 'NONE', *, *, #8089, .F. ) ;
#14637 = AXIS2_PLACEMENT_3D ( 'NONE', #11093, #14033, #519 ) ;
#14638 = CARTESIAN_POINT ( 'NONE',  ( 41.58830220609386430, 56.99948385550241170, 0.02388180880523263147 ) ) ;
#14639 = PRODUCT_DEFINITION ( 'UNKNOWN', '', #17648, #17956 ) ;
#14640 = CARTESIAN_POINT ( 'NONE',  ( 0.000000000000000000, 3.031088913245533867, 1.750000000000002887 ) ) ;
#14641 = VECTOR ( 'NONE', #11081, 1000.000000000000114 ) ;
#14642 = CARTESIAN_POINT ( 'NONE',  ( 55.69932041026404335, 49.89948385550241028, -1.875703265242203432 ) ) ;
#14643 = DIRECTION ( 'NONE',  ( 1.000000000000000000, 0.000000000000000000, 0.000000000000000000 ) ) ;
#14644 = CARTESIAN_POINT ( 'NONE',  ( -17.79870116617242459, -29.12174527145394265, 0.000000000000000000 ) ) ;
#14645 = CARTESIAN_POINT ( 'NONE',  ( 47.37792948025170858, 49.60051614449766788, 7.992620115222797139 ) ) ;
#14646 = EDGE_CURVE ( 'NONE', #2011, #15477, #11785, .T. ) ;
#14647 = CARTESIAN_POINT ( 'NONE',  ( 53.54508667620424234, 46.70051614449766220, -4.840751629271188961 ) ) ;
#14648 = FACE_OUTER_BOUND ( 'NONE', #3679, .T. ) ;
#14649 = LINE ( 'NONE', #15053, #1263 ) ;
#14650 = VERTEX_POINT ( 'NONE', #10213 ) ;
#14651 = EDGE_CURVE ( 'NONE', #3811, #13420, #19081, .T. ) ;
#14652 = ADVANCED_FACE ( 'NONE', ( #14833 ), #14627, .T. ) ;
#14653 = ORIENTED_EDGE ( 'NONE', *, *, #17208, .F. ) ;
#14654 = CARTESIAN_POINT ( 'NONE',  ( 2.449293598294706513E-15, -20.00000000000000000, 9.000000000000000000 ) ) ;
#14655 = VERTEX_POINT ( 'NONE', #4062 ) ;
#14656 = VECTOR ( 'NONE', #17746, 1000.000000000000000 ) ;
#14657 = AXIS2_PLACEMENT_3D ( 'NONE', #7435, #11737, #5674 ) ;
#14658 = CARTESIAN_POINT ( 'NONE',  ( -0.1085714285714285687, -3.798448662927795372, -0.8000000000000000444 ) ) ;
#14659 = DIRECTION ( 'NONE',  ( -1.000000000000000000, 1.734723475976807094E-16, 0.000000000000000000 ) ) ;
#14660 = APPLICATION_CONTEXT ( 'automotive_design' ) ;
#14661 = ORIENTED_EDGE ( 'NONE', *, *, #10804, .T. ) ;
#14662 = VERTEX_POINT ( 'NONE', #1215 ) ;
#14663 = DIRECTION ( 'NONE',  ( 0.000000000000000000, 0.000000000000000000, 1.000000000000000000 ) ) ;
#14664 = EDGE_CURVE ( 'NONE', #16610, #18021, #13441, .T. ) ;
#14665 = CARTESIAN_POINT ( 'NONE',  ( 47.74827507625477807, 46.59948385550239180, 7.007379884777229506 ) ) ;
#14666 = EDGE_CURVE ( 'NONE', #18444, #1643, #11871, .T. ) ;
#14667 = ORIENTED_EDGE ( 'NONE', *, *, #13098, .F. ) ;
#14668 = DIRECTION ( 'NONE',  ( 1.000000000000000000, 0.000000000000000000, 0.000000000000000000 ) ) ;
#14669 = ORIENTED_EDGE ( 'NONE', *, *, #16411, .T. ) ;
#14670 = CARTESIAN_POINT ( 'NONE',  ( -4.236525694536558362, 2.416953475386465211, -3.751298745799836354 ) ) ;
#14671 = CARTESIAN_POINT ( 'NONE',  ( 55.96859303347804371, 50.19948385550240744, 4.306917132069425946 ) ) ;
#14672 = CARTESIAN_POINT ( 'NONE',  ( 1.219878473194462964, -24.84890673354692936, 15.00000000000000355 ) ) ;
#14673 = CARTESIAN_POINT ( 'NONE',  ( 49.97728705011495265, 49.50051614449765935, 7.000000000000000888 ) ) ;
#14674 = CARTESIAN_POINT ( 'NONE',  ( -20.63749999999999929, 0.000000000000000000, -4.599999999999999645 ) ) ;
#14675 = AXIS2_PLACEMENT_3D ( 'NONE', #9770, #9663, #6728 ) ;
#14676 = EDGE_CURVE ( 'NONE', #1031, #13632, #6556, .T. ) ;
#14677 = AXIS2_PLACEMENT_3D ( 'NONE', #16947, #6251, #181 ) ;
#14678 = CARTESIAN_POINT ( 'NONE',  ( -1.250000000000000000, -6.429618962271402616, 0.000000000000000000 ) ) ;
#14679 = ADVANCED_FACE ( 'NONE', ( #1775 ), #5622, .T. ) ;
#14680 = CARTESIAN_POINT ( 'NONE',  ( 6.244297270354684848, -1.798312406574552930E-11, -5.105276777067894400 ) ) ;
#14681 = SHAPE_REPRESENTATION ( 'hub', ( #10359 ), #8423 ) ;
#14682 = EDGE_CURVE ( 'NONE', #9693, #8618, #11493, .T. ) ;
#14683 = ORIENTED_EDGE ( 'NONE', *, *, #13168, .T. ) ;
#14684 = ORIENTED_EDGE ( 'NONE', *, *, #14827, .F. ) ;
#14685 = FACE_OUTER_BOUND ( 'NONE', #8906, .T. ) ;
#14686 = CARTESIAN_POINT ( 'NONE',  ( 0.000000000000000000, 0.000000000000000000, 0.000000000000000000 ) ) ;
#14687 = CARTESIAN_POINT ( 'NONE',  ( 2.449293598294706513E-15, -20.00000000000000000, 9.999999999999998224 ) ) ;
#14688 = ORIENTED_EDGE ( 'NONE', *, *, #9283, .F. ) ;
#14689 = CARTESIAN_POINT ( 'NONE',  ( 54.89903213687075834, 44.74560054925188268, -5.000000000000007105 ) ) ;
#14690 = AXIS2_PLACEMENT_3D ( 'NONE', #829, #2313, #2413 ) ;
#14691 = AXIS2_PLACEMENT_3D ( 'NONE', #5725, #19187, #16029 ) ;
#14692 = ORIENTED_EDGE ( 'NONE', *, *, #1853, .T. ) ;
#14693 = VERTEX_POINT ( 'NONE', #6279 ) ;
#14694 = DIRECTION ( 'NONE',  ( 1.000000000000000000, 0.000000000000000000, 0.000000000000000000 ) ) ;
#14695 = CARTESIAN_POINT ( 'NONE',  ( 43.69122665457040000, 50.00051614449765935, -0.02388180880515696977 ) ) ;
#14696 = CARTESIAN_POINT ( 'NONE',  ( 0.1983443223721600701, -5.300482436767282479, -0.8192951148925879945 ) ) ;
#14697 = CARTESIAN_POINT ( 'NONE',  ( -14.00000000000000000, 15.00000000000001599, 9.000000000000000000 ) ) ;
#14698 = CARTESIAN_POINT ( 'NONE',  ( 44.91013252490152752, 48.79948385550240175, 3.727524721679198461 ) ) ;
#14699 = CARTESIAN_POINT ( 'NONE',  ( 4.175648173966055587, -2.207990556236547608, -3.469390959564065291 ) ) ;
#14700 = CARTESIAN_POINT ( 'NONE',  ( 50.02271294988512551, 50.49948385550240459, 7.000000000000000888 ) ) ;
#14701 = AXIS2_PLACEMENT_3D ( 'NONE', #608, #11377, #2389 ) ;
#14702 = CARTESIAN_POINT ( 'NONE',  ( 45.27934281921082516, 45.70051614449766220, 6.458785618021089192 ) ) ;
#14703 = CARTESIAN_POINT ( 'NONE',  ( 4.165266963751721008, -2.049631966911996006, -3.550066703508900190 ) ) ;
#14704 = ORIENTED_EDGE ( 'NONE', *, *, #10466, .F. ) ;
#14705 = DIRECTION ( 'NONE',  ( 1.000000000000000000, 0.000000000000000000, 0.000000000000000000 ) ) ;
#14706 = ADVANCED_FACE ( 'NONE', ( #4814 ), #9585, .T. ) ;
#14707 = B_SPLINE_CURVE_WITH_KNOTS ( 'NONE', 3,
 ( #14262, #8584, #15653, #2331, #14554, #6628 ),
 .UNSPECIFIED., .F., .F.,
 ( 4, 2, 4 ),
 ( 0.000000000000000000, 0.0002095117440854740156, 0.0004190234881709480313 ),
 .UNSPECIFIED. ) ;
#14708 = APPLICATION_PROTOCOL_DEFINITION ( 'draft international standard', 'automotive_design', 1998, #13412 ) ;
#14709 = VECTOR ( 'NONE', #12806, 1000.000000000000000 ) ;
#14710 = ORIENTED_EDGE ( 'NONE', *, *, #7900, .F. ) ;
#14711 = CARTESIAN_POINT ( 'NONE',  ( -1.287237434361707233, -3.875615274277397937, -3.430618716626816500 ) ) ;
#14712 = ADVANCED_FACE ( 'NONE', ( #15295 ), #12503, .T. ) ;
#14713 = DIRECTION ( 'NONE',  ( 9.858538378746663627E-23, -5.031452844637890958E-23, 1.000000000000000000 ) ) ;
#14714 = AXIS2_PLACEMENT_3D ( 'NONE', #1781, #12163, #9127 ) ;
#14715 = CYLINDRICAL_SURFACE ( 'NONE', #8441, 5.000000000000007994 ) ;
#14716 = CARTESIAN_POINT ( 'NONE',  ( 6.196878017913833858, 5.292377467571573568, 0.8333333333333322601 ) ) ;
#14717 = AXIS2_PLACEMENT_3D ( 'NONE', #8919, #1379, #17861 ) ;
#14718 = CARTESIAN_POINT ( 'NONE',  ( 2.649999999999988365, 15.00000000000001599, 9.999999999999998224 ) ) ;
#14719 = CIRCLE ( 'NONE', #6894, 1.000000000000000000 ) ;
#14720 = CYLINDRICAL_SURFACE ( 'NONE', #11718, 7.000000000000000000 ) ;
#14721 = DIRECTION ( 'NONE',  ( -0.04542589977017699732, 0.9989677110047501252, 0.000000000000000000 ) ) ;
#14722 = CARTESIAN_POINT ( 'NONE',  ( 45.86712807150323812, 49.29948385550240175, -5.649768623646098220 ) ) ;
#14723 = CIRCLE ( 'NONE', #19158, 3.299999999999999822 ) ;
#14724 = DIRECTION ( 'NONE',  ( 0.9999419836444144449, 0.01077169184824096695, 0.000000000000000000 ) ) ;
#14725 = CARTESIAN_POINT ( 'NONE',  ( 57.60143344285433642, 53.89948385550240317, -2.493737253992118319 ) ) ;
#14726 = CARTESIAN_POINT ( 'NONE',  ( 19.02113032590313679, -26.18033988749876428, -9.000000000000000000 ) ) ;
#14727 = CARTESIAN_POINT ( 'NONE',  ( 47.70284917648459100, 47.60051614449763946, 6.992620115222796251 ) ) ;
#14728 = LINE ( 'NONE', #14624, #5980 ) ;
#14729 = AXIS2_PLACEMENT_3D ( 'NONE', #495, #15694, #2275 ) ;
#14730 = EDGE_LOOP ( 'NONE', ( #4481, #924, #14732, #16833 ) ) ;
#14731 = VECTOR ( 'NONE', #3090, 1000.000000000000000 ) ;
#14732 = ORIENTED_EDGE ( 'NONE', *, *, #10215, .T. ) ;
#14733 = CARTESIAN_POINT ( 'NONE',  ( 2.449293598294706513E-15, -20.00000000000000000, -9.000000000000000000 ) ) ;
#14734 = ORIENTED_EDGE ( 'NONE', *, *, #15610, .F. ) ;
#14735 = DIRECTION ( 'NONE',  ( -1.000000000000000000, 0.000000000000000000, 0.000000000000000000 ) ) ;
#14736 = AXIS2_PLACEMENT_3D ( 'NONE', #18955, #11274, #5112 ) ;
#14737 = ORIENTED_EDGE ( 'NONE', *, *, #14215, .T. ) ;
#14738 = DIRECTION ( 'NONE',  ( -0.000000000000000000, -0.000000000000000000, 1.000000000000000000 ) ) ;
#14739 = ORIENTED_EDGE ( 'NONE', *, *, #5310, .T. ) ;
#14740 = CARTESIAN_POINT ( 'NONE',  ( 0.6507732100473444525, -4.243078065514795050, -0.2236248678334952777 ) ) ;
#14741 = ORIENTED_EDGE ( 'NONE', *, *, #7944, .T. ) ;
#14742 = CARTESIAN_POINT ( 'NONE',  ( 57.60143344285433642, 57.89948385550241028, -2.493737253992118319 ) ) ;
#14743 = CARTESIAN_POINT ( 'NONE',  ( 0.02993401039713550899, 2.688325911136453250, -2.343682934607766111 ) ) ;
#14744 = CARTESIAN_POINT ( 'NONE',  ( 46.49166364869460466, 58.69948385550240033, 4.867452303228209765 ) ) ;
#14745 = DIRECTION ( 'NONE',  ( -0.000000000000000000, -0.000000000000000000, 1.000000000000000000 ) ) ;
#14746 = DIRECTION ( 'NONE',  ( -0.6520673188974834833, 0.7581610723493046322, 1.805535875966852419E-17 ) ) ;
#14747 = VECTOR ( 'NONE', #13011, 1000.000000000000000 ) ;
#14748 = AXIS2_PLACEMENT_3D ( 'NONE', #3379, #3201, #13762 ) ;
#14749 = CARTESIAN_POINT ( 'NONE',  ( 41.58830220609386430, 46.00051614449764514, -0.02388180880514929535 ) ) ;
#14750 = CARTESIAN_POINT ( 'NONE',  ( 44.30067958973594955, 50.10051614449766078, -1.875703265242155693 ) ) ;
#14751 = DIRECTION ( 'NONE',  ( 1.000000000000000000, 0.000000000000000000, 0.000000000000000000 ) ) ;
#14752 = CARTESIAN_POINT ( 'NONE',  ( 1.150000000000000577, 0.000000000000000000, 0.000000000000000000 ) ) ;
#14753 = EDGE_CURVE ( 'NONE', #15143, #17997, #5181, .T. ) ;
#14754 = ORIENTED_EDGE ( 'NONE', *, *, #6389, .F. ) ;
#14755 = ORIENTED_EDGE ( 'NONE', *, *, #16480, .T. ) ;
#14756 = CARTESIAN_POINT ( 'NONE',  ( -4.000000000000000000, -2.309401076758515803, -0.4999999999999995559 ) ) ;
#14757 = ORIENTED_EDGE ( 'NONE', *, *, #14753, .F. ) ;
#14758 = FACE_OUTER_BOUND ( 'NONE', #6225, .T. ) ;
#14759 = DIRECTION ( 'NONE',  ( 0.000000000000000000, -1.073081856240829552E-16, -1.000000000000000000 ) ) ;
#14760 = VECTOR ( 'NONE', #5396, 1000.000000000000114 ) ;
#14761 = ORIENTED_EDGE ( 'NONE', *, *, #12881, .F. ) ;
#14762 = CARTESIAN_POINT ( 'NONE',  ( -155.0676494111543491, -18.79939778875158396, -15.79999999999999893 ) ) ;
#14763 = CARTESIAN_POINT ( 'NONE',  ( 55.94051828345050836, 47.79948385550240886, -4.345558710429103577 ) ) ;
#14764 = VECTOR ( 'NONE', #2607, 1000.000000000000114 ) ;
#14765 = VERTEX_POINT ( 'NONE', #15685 ) ;
#14766 = DIRECTION ( 'NONE',  ( -1.000000000000000000, -0.000000000000000000, -0.000000000000000000 ) ) ;
#14767 = ORIENTED_EDGE ( 'NONE', *, *, #14193, .T. ) ;
#14768 = CARTESIAN_POINT ( 'NONE',  ( 10.93224627749321876, -36.74771600333119181, 9.000000000000000000 ) ) ;
#14769 = CARTESIAN_POINT ( 'NONE',  ( 54.09612160359786515, 53.69948385550240744, -5.676469297603166098 ) ) ;
#14770 = CARTESIAN_POINT ( 'NONE',  ( -155.0676494111543491, -18.79939778875158396, -15.79999999999999893 ) ) ;
#14771 = EDGE_CURVE ( 'NONE', #5073, #6996, #11063, .T. ) ;
#14772 = CARTESIAN_POINT ( 'NONE',  ( 55.94051828345053679, 49.20051614449766930, 4.345558710429044069 ) ) ;
#14773 = LINE ( 'NONE', #1452, #1381 ) ;
#14774 = DIRECTION ( 'NONE',  ( 0.000000000000000000, 0.000000000000000000, 1.000000000000000000 ) ) ;
#14775 = CARTESIAN_POINT ( 'NONE',  ( -154.9999999999999716, -14.99999999999999645, 15.00000000000000000 ) ) ;
#14776 = VERTEX_POINT ( 'NONE', #8022 ) ;
#14777 = EDGE_CURVE ( 'NONE', #12892, #2842, #3442, .T. ) ;
#14778 = PRODUCT_DEFINITION_SHAPE ( 'NONE', 'NONE',  #8787 ) ;
#14779 = EDGE_CURVE ( 'NONE', #7129, #19088, #16876, .T. ) ;
#14780 = ORIENTED_EDGE ( 'NONE', *, *, #4368, .T. ) ;
#14781 = ORIENTED_EDGE ( 'NONE', *, *, #569, .T. ) ;
#14782 = CARTESIAN_POINT ( 'NONE',  ( -1.144235203016679359, -3.958177651039096911, -0.09382832055446428676 ) ) ;
#14783 = SHAPE_REPRESENTATION_RELATIONSHIP ( 'NONE' , 'NONE' ,  #11935, #15256 ) ;
#14784 = EDGE_CURVE ( 'NONE', #9062, #16469, #3623, .T. ) ;
#14785 = CARTESIAN_POINT ( 'NONE',  ( 56.66441430157296821, 48.09948385550240602, 2.141517661632100111 ) ) ;
#14786 = DIRECTION ( 'NONE',  ( -1.000000000000000000, 1.734723475976807094E-16, 0.000000000000000000 ) ) ;
#14787 = ORIENTED_EDGE ( 'NONE', *, *, #17573, .F. ) ;
#14788 = DIRECTION ( 'NONE',  ( -0.6520673188974834833, 0.7581610723493047432, 1.805535875966851803E-17 ) ) ;
#14789 = EDGE_CURVE ( 'NONE', #17065, #4767, #7504, .T. ) ;
#14790 = CIRCLE ( 'NONE', #7582, 4.799999999999999822 ) ;
#14791 = EDGE_LOOP ( 'NONE', ( #1445, #1214 ) ) ;
#14792 = EDGE_LOOP ( 'NONE', ( #12011, #1966 ) ) ;
#14793 = CARTESIAN_POINT ( 'NONE',  ( 0.000000000000000000, 20.00000000000001421, 9.999999999999998224 ) ) ;
#14794 = UNCERTAINTY_MEASURE_WITH_UNIT (LENGTH_MEASURE( 1.000000000000000082E-05 ), #11448, 'distance_accuracy_value', 'NONE');
#14795 = DIRECTION ( 'NONE',  ( 0.000000000000000000, 0.000000000000000000, 1.000000000000000000 ) ) ;
#14796 = CARTESIAN_POINT ( 'NONE',  ( 53.54508667620424234, 48.70051614449766930, -4.840751629271188961 ) ) ;
#14797 = CARTESIAN_POINT ( 'NONE',  ( 2.449293598294706513E-15, -20.00000000000000000, 9.000000000000000000 ) ) ;
#14798 = SURFACE_SIDE_STYLE ('',( #16288 ) ) ;
#14799 = CARTESIAN_POINT ( 'NONE',  ( 46.49166364869460466, 60.69948385550240033, 4.867452303228209765 ) ) ;
#14800 = CARTESIAN_POINT ( 'NONE',  ( 50.00000000000000000, 40.00000000000000000, 0.000000000000000000 ) ) ;
#14801 = CARTESIAN_POINT ( 'NONE',  ( 52.25172492374522903, 55.59948385550241312, -7.007379884777225953 ) ) ;
#14802 = EDGE_CURVE ( 'NONE', #14841, #5461, #17849, .T. ) ;
#14803 = CARTESIAN_POINT ( 'NONE',  ( 47.42335538002180328, 52.40051614449767214, -8.007379884777206414 ) ) ;
#14804 = CARTESIAN_POINT ( 'NONE',  ( -2.000000000000002665, -3.464101615137770374, -3.142992957459237680 ) ) ;
#14805 = CARTESIAN_POINT ( 'NONE',  ( 3.806834918298644954, -3.031088913245536975, 1.750000000000000666 ) ) ;
#14806 = EDGE_CURVE ( 'NONE', #16928, #4766, #13999, .T. ) ;
#14807 = ADVANCED_BREP_SHAPE_REPRESENTATION ( '', ( #2264, #10359 ), #3416 ) ;
#14808 = LINE ( 'NONE', #13438, #6825 ) ;
#14809 = FILL_AREA_STYLE_COLOUR ( '', #8799 ) ;
#14810 = DIRECTION ( 'NONE',  ( 2.191393683118470056E-17, 7.538405132783724027E-17, 1.000000000000000000 ) ) ;
#14811 = PRODUCT_DEFINITION_FORMATION_WITH_SPECIFIED_SOURCE ( 'ANY', '', #3649, .NOT_KNOWN. ) ;
#14812 = ORIENTED_EDGE ( 'NONE', *, *, #19295, .T. ) ;
#14813 = PLANE ( 'NONE',  #11417 ) ;
#14814 = CARTESIAN_POINT ( 'NONE',  ( 1.267864665251833278E-11, -20.00000000000000000, 9.000000000000000000 ) ) ;
#14815 = MANIFOLD_SOLID_BREP ( 'M5 Clearance Hole1', #7100 ) ;
#14816 = FACE_OUTER_BOUND ( 'NONE', #4697, .T. ) ;
#14817 = CARTESIAN_POINT ( 'NONE',  ( 6.367873360227558344, 5.773502691896261751, 0.000000000000000000 ) ) ;
#14818 = DIRECTION ( 'NONE',  ( 0.000000000000000000, -0.000000000000000000, 1.000000000000000000 ) ) ;
#14819 = FACE_OUTER_BOUND ( 'NONE', #6700, .T. ) ;
#14820 = LINE ( 'NONE', #16501, #15575 ) ;
#14821 = CARTESIAN_POINT ( 'NONE',  ( 43.34962307344081012, 56.89948385550240317, 2.184720259617164650 ) ) ;
#14822 = CYLINDRICAL_SURFACE ( 'NONE', #5688, 5.000000000000000888 ) ;
#14823 = CARTESIAN_POINT ( 'NONE',  ( 58.41169779390614281, 55.99948385550241170, -0.02388180880523160798 ) ) ;
#14824 = CARTESIAN_POINT ( 'NONE',  ( 4.030867648404857562, -3.732851566702167556, -0.5345114293585713217 ) ) ;
#14825 = EDGE_CURVE ( 'NONE', #12888, #7410, #11846, .T. ) ;
#14826 = CARTESIAN_POINT ( 'NONE',  ( 56.66441430157294690, 48.90051614449766504, -2.141517661632166281 ) ) ;
#14827 = EDGE_CURVE ( 'NONE', #17459, #14529, #4904, .T. ) ;
#14828 = PLANE ( 'NONE',  #1599 ) ;
#14829 = ORIENTED_EDGE ( 'NONE', *, *, #16944, .T. ) ;
#14830 = TOROIDAL_SURFACE ( 'NONE', #6695, 5.384454397937118664, 0.5155456020628804703 ) ;
#14831 = EDGE_CURVE ( 'NONE', #7722, #8295, #3713, .T. ) ;
#14832 = ORIENTED_EDGE ( 'NONE', *, *, #3794, .F. ) ;
#14833 = FACE_OUTER_BOUND ( 'NONE', #5978, .T. ) ;
#14834 = EDGE_LOOP ( 'NONE', ( #9806, #15339, #6900, #1843, #10687 ) ) ;
#14835 = VECTOR ( 'NONE', #15522, 1000.000000000000000 ) ;
#14836 = CARTESIAN_POINT ( 'NONE',  ( 20.00000000000000000, -20.00000000000000000, -23.00000000000000000 ) ) ;
#14837 = EDGE_LOOP ( 'NONE', ( #932, #3134, #421, #11059 ) ) ;
#14838 = FACE_OUTER_BOUND ( 'NONE', #19067, .T. ) ;
#14839 = VERTEX_POINT ( 'NONE', #3922 ) ;
#14840 = CARTESIAN_POINT ( 'NONE',  ( 30.00000000000000355, -40.00000000000000000, 10.00000000000000000 ) ) ;
#14841 = VERTEX_POINT ( 'NONE', #8222 ) ;
#14842 = LINE ( 'NONE', #13371, #17445 ) ;
#14843 = FACE_OUTER_BOUND ( 'NONE', #6848, .T. ) ;
#14844 = EDGE_CURVE ( 'NONE', #17411, #3719, #15878, .T. ) ;
#14845 = CARTESIAN_POINT ( 'NONE',  ( 56.30877334542961421, 53.99948385550241170, -0.02388180880520959434 ) ) ;
#14846 = VECTOR ( 'NONE', #2194, 1000.000000000000000 ) ;
#14847 = DIRECTION ( 'NONE',  ( 1.000000000000000000, 1.387778780781445676E-16, 0.000000000000000000 ) ) ;
#14848 = DIRECTION ( 'NONE',  ( 0.000000000000000000, 0.000000000000000000, 1.000000000000000000 ) ) ;
#14849 = CARTESIAN_POINT ( 'NONE',  ( 54.68390685589039890, 53.30051614449767072, 6.485486291978072693 ) ) ;
#14850 = CIRCLE ( 'NONE', #3588, 4.000000000000021316 ) ;
#14851 = EDGE_CURVE ( 'NONE', #62, #4248, #981, .T. ) ;
#14852 = CARTESIAN_POINT ( 'NONE',  ( 53.50833635130544508, 47.30051614449766362, 4.867452303228181343 ) ) ;
#14853 = DIRECTION ( 'NONE',  ( -0.000000000000000000, 0.000000000000000000, -1.000000000000000000 ) ) ;
#14854 = CARTESIAN_POINT ( 'NONE',  ( -0.6666666666666651864, 4.233901974057260098, -3.300726591567081147 ) ) ;
#14855 = ORIENTED_EDGE ( 'NONE', *, *, #10471, .F. ) ;
#14856 = VERTEX_POINT ( 'NONE', #1171 ) ;
#14857 = ORIENTED_EDGE ( 'NONE', *, *, #5792, .F. ) ;
#14858 = CARTESIAN_POINT ( 'NONE',  ( -74.99999999999997158, -39.99999999999998579, 10.00000000000000000 ) ) ;
#14859 = CARTESIAN_POINT ( 'NONE',  ( 4.000000000000001776, 0.000000000000000000, -2.200000000000001066 ) ) ;
#14860 = ORIENTED_EDGE ( 'NONE', *, *, #14103, .T. ) ;
#14861 = CIRCLE ( 'NONE', #19291, 4.000000000000000000 ) ;
#14862 = DIRECTION ( 'NONE',  ( -0.000000000000000000, -0.000000000000000000, 1.000000000000000000 ) ) ;
#14863 = CARTESIAN_POINT ( 'NONE',  ( 45.86712807150323812, 47.29948385550240886, -5.649768623646098220 ) ) ;
#14864 = VERTEX_POINT ( 'NONE', #8615 ) ;
#14865 = DIRECTION ( 'NONE',  ( 0.000000000000000000, 0.000000000000000000, 1.000000000000000000 ) ) ;
#14866 = ORIENTED_EDGE ( 'NONE', *, *, #13030, .T. ) ;
#14867 = CARTESIAN_POINT ( 'NONE',  ( -8.134732861515892921, -38.27090915285207018, -9.000000000000000000 ) ) ;
#14868 = CIRCLE ( 'NONE', #3286, 4.000000000000003553 ) ;
#14869 = CARTESIAN_POINT ( 'NONE',  ( 55.94051828345050836, 59.79948385550238754, -4.345558710429104465 ) ) ;
#14870 = DIRECTION ( 'NONE',  ( -0.000000000000000000, -0.000000000000000000, 1.000000000000000000 ) ) ;
#14871 = CARTESIAN_POINT ( 'NONE',  ( 44.05948171654945611, 54.20051614449764799, -4.345558710429044069 ) ) ;
#14872 = CARTESIAN_POINT ( 'NONE',  ( 11.75570504584960041, -36.18033988749885310, 9.000000000000000000 ) ) ;
#14873 = CARTESIAN_POINT ( 'NONE',  ( 19.02113032590300890, -13.81966011250085025, 9.000000000000000000 ) ) ;
#14874 = CIRCLE ( 'NONE', #2991, 2.500000000000000444 ) ;
#14875 = FACE_OUTER_BOUND ( 'NONE', #15716, .T. ) ;
#14876 = VERTEX_POINT ( 'NONE', #4114 ) ;
#14877 = VECTOR ( 'NONE', #16554, 1000.000000000000000 ) ;
#14878 = ORIENTED_EDGE ( 'NONE', *, *, #11670, .T. ) ;
#14879 = ORIENTED_EDGE ( 'NONE', *, *, #7525, .F. ) ;
#14880 = CYLINDRICAL_SURFACE ( 'NONE', #3097, 5.000000000000000888 ) ;
#14881 = AXIS2_PLACEMENT_3D ( 'NONE', #1973, #15483, #14198 ) ;
#14882 = CARTESIAN_POINT ( 'NONE',  ( 52.57664461997811856, 63.59948385550239891, -8.007379884777229506 ) ) ;
#14883 = CARTESIAN_POINT ( 'NONE',  ( -154.9999999999999716, -14.99999999999999645, -15.79999999999999893 ) ) ;
#14884 = ORIENTED_EDGE ( 'NONE', *, *, #7166, .F. ) ;
#14885 = CARTESIAN_POINT ( 'NONE',  ( 6.436591462021357124, 5.789018756751930894, -2.883547477572278442E-16 ) ) ;
#14886 = ORIENTED_EDGE ( 'NONE', *, *, #8928, .T. ) ;
#14887 = CARTESIAN_POINT ( 'NONE',  ( 56.65037692655921120, 61.10051614449766078, 2.184720259617097593 ) ) ;
#14888 = ORIENTED_EDGE ( 'NONE', *, *, #19157, .F. ) ;
#14889 = APPLICATION_CONTEXT ( 'automotive_design' ) ;
#14890 = EDGE_CURVE ( 'NONE', #6396, #11089, #19392, .T. ) ;
#14891 = CARTESIAN_POINT ( 'NONE',  ( 1.654252653721905331, 3.663718938583014229, -0.01223254789873410957 ) ) ;
#14892 = CARTESIAN_POINT ( 'NONE',  ( 2.000000000000000000, 0.8865213383406680414, -1.535500000000000975 ) ) ;
#14893 = PRODUCT_RELATED_PRODUCT_CATEGORY ( 'part', '', ( #14273 ) ) ;
#14894 = CARTESIAN_POINT ( 'NONE',  ( 44.91013252490150620, 46.20051614449766220, -3.727524721679154940 ) ) ;
#14895 = DIRECTION ( 'NONE',  ( 1.000000000000000000, 0.000000000000000000, 0.000000000000000000 ) ) ;
#14896 = AXIS2_PLACEMENT_3D ( 'NONE', #16470, #16377, #17847 ) ;
#14897 = EDGE_CURVE ( 'NONE', #16610, #11107, #13027, .T. ) ;
#14898 = DIRECTION ( 'NONE',  ( 1.000000000000000000, -6.938893903907227392E-16, 0.000000000000000000 ) ) ;
#14899 = CARTESIAN_POINT ( 'NONE',  ( 43.69122665457040000, 58.99948385550239749, 0.02388180880521036456 ) ) ;
#14900 = CARTESIAN_POINT ( 'NONE',  ( 1.243802165048773611, -3.900692638707475624, -3.223146290109810241 ) ) ;
#14901 = CARTESIAN_POINT ( 'NONE',  ( 42.63976443033212860, 50.99948385550240459, 0.02388180880522514787 ) ) ;
#14902 = CARTESIAN_POINT ( 'NONE',  ( 52.57664461997821093, 53.40051614449765793, 8.007379884777206414 ) ) ;
#14903 = EDGE_CURVE ( 'NONE', #666, #3752, #2463, .T. ) ;
#14904 = CARTESIAN_POINT ( 'NONE',  ( 0.1739375980333740523, -5.301268757141563093, 0.8179331680533010740 ) ) ;
#14905 = EDGE_CURVE ( 'NONE', #9070, #273, #14018, .T. ) ;
#14906 = LINE ( 'NONE', #4429, #16807 ) ;
#14907 = PRESENTATION_LAYER_ASSIGNMENT (  '', '', ( #9556 ) ) ;
#14908 = CARTESIAN_POINT ( 'NONE',  ( -2.000000000000000000, -6.429618962271402616, -1.000000000000000000 ) ) ;
#14909 = EDGE_CURVE ( 'NONE', #12622, #6955, #14346, .T. ) ;
#14910 = APPLICATION_PROTOCOL_DEFINITION ( 'draft international standard', 'automotive_design', 1998, #6286 ) ;
#14911 = ORIENTED_EDGE ( 'NONE', *, *, #934, .F. ) ;
#14912 = CARTESIAN_POINT ( 'NONE',  ( -1.250000000000000666, 5.575000000000000178, 0.000000000000000000 ) ) ;
#14913 = DIRECTION ( 'NONE',  ( 0.000000000000000000, 0.000000000000000000, 1.000000000000000000 ) ) ;
#14914 = ADVANCED_FACE ( 'NONE', ( #6951 ), #5577, .F. ) ;
#14915 = MANIFOLD_SOLID_BREP ( 'Notch', #12109 ) ;
#14916 = CARTESIAN_POINT ( 'NONE',  ( 43.34962307344081012, 62.89948385550241028, 2.184720259617164650 ) ) ;
#14917 = EDGE_CURVE ( 'NONE', #17135, #3297, #13408, .T. ) ;
#14918 = DIRECTION ( 'NONE',  ( 0.6691306063588675634, -0.7431448254773859174, 0.000000000000000000 ) ) ;
#14919 = FACE_OUTER_BOUND ( 'NONE', #16739, .T. ) ;
#14920 = CYLINDRICAL_SURFACE ( 'NONE', #3680, 1.000000000000000888 ) ;
#14921 = CARTESIAN_POINT ( 'NONE',  ( 47.70284917648453415, 59.39948385550241028, -6.992620115222774047 ) ) ;
#14922 = LINE ( 'NONE', #7761, #4821 ) ;
#14923 = CIRCLE ( 'NONE', #516, 4.000000000000021316 ) ;
#14924 = CARTESIAN_POINT ( 'NONE',  ( 54.72065718078924590, 52.29948385550240886, 6.458785618021043895 ) ) ;
#14925 = CARTESIAN_POINT ( 'NONE',  ( 4.180345304246199767, -4.135116856707399258, 0.02129519942689610257 ) ) ;
#14926 = CARTESIAN_POINT ( 'NONE',  ( 43.33558569842706021, 57.90051614449766504, 2.141517661632167169 ) ) ;
#14927 = CARTESIAN_POINT ( 'NONE',  ( 0.000000000000000000, 0.000000000000000000, 0.000000000000000000 ) ) ;
#14928 = ORIENTED_EDGE ( 'NONE', *, *, #4146, .F. ) ;
#14929 = ORIENTED_EDGE ( 'NONE', *, *, #15493, .F. ) ;
#14930 = ORIENTED_EDGE ( 'NONE', *, *, #886, .F. ) ;
#14931 = VECTOR ( 'NONE', #2619, 1000.000000000000000 ) ;
#14932 = PLANE ( 'NONE',  #418 ) ;
#14933 = VECTOR ( 'NONE', #4983, 1000.000000000000000 ) ;
#14934 = ORIENTED_EDGE ( 'NONE', *, *, #2382, .F. ) ;
#14935 = CARTESIAN_POINT ( 'NONE',  ( 4.078421086530217288, -3.990950201428958621, -1.000000000000000000 ) ) ;
#14936 = ORIENTED_EDGE ( 'NONE', *, *, #8789, .T. ) ;
#14937 = DIRECTION ( 'NONE',  ( 0.000000000000000000, -1.000000000000000000, 8.673617379884035472E-16 ) ) ;
#14938 = ORIENTED_EDGE ( 'NONE', *, *, #13050, .T. ) ;
#14939 = FACE_OUTER_BOUND ( 'NONE', #8806, .T. ) ;
#14940 = DIRECTION ( 'NONE',  ( 0.000000000000000000, 0.000000000000000000, -1.000000000000000000 ) ) ;
#14941 = CARTESIAN_POINT ( 'NONE',  ( 48.07319477248768180, 56.59948385550239891, 6.007379884777225953 ) ) ;
#14942 = CARTESIAN_POINT ( 'NONE',  ( -154.9999999999999716, -14.99999999999999645, -15.00000000000000000 ) ) ;
#14943 = CARTESIAN_POINT ( 'NONE',  ( -18.68843350152489080, -27.12337372732064011, 0.000000000000000000 ) ) ;
#14944 = CARTESIAN_POINT ( 'NONE',  ( 43.20883090819742023, 56.20051614449766220, -4.963592699178938972 ) ) ;
#14945 = CARTESIAN_POINT ( 'NONE',  ( 46.49166364869456913, 58.30051614449765651, -4.867452303228181343 ) ) ;
#14946 = VECTOR ( 'NONE', #2079, 1000.000000000000000 ) ;
#14947 = CARTESIAN_POINT ( 'NONE',  ( -154.9999999999999716, -23.00000000000000000, 15.00000000000000000 ) ) ;
#14948 = MECHANICAL_DESIGN_GEOMETRIC_PRESENTATION_REPRESENTATION (  '', ( #3073 ), #7440 ) ;
#14949 = DIRECTION ( 'NONE',  ( -0.000000000000000000, -0.000000000000000000, 1.000000000000000000 ) ) ;
#14950 = EDGE_LOOP ( 'NONE', ( #14857, #15363, #7392, #17268 ) ) ;
#14951 = ORIENTED_EDGE ( 'NONE', *, *, #8951, .T. ) ;
#14952 = FACE_OUTER_BOUND ( 'NONE', #11627, .T. ) ;
#14953 = ORIENTED_EDGE ( 'NONE', *, *, #11609, .T. ) ;
#14954 = EDGE_CURVE ( 'NONE', #15438, #18021, #3827, .T. ) ;
#14955 = CARTESIAN_POINT ( 'NONE',  ( 52.25172492374522903, 63.59948385550237759, -7.007379884777225953 ) ) ;
#14956 =( NAMED_UNIT ( * ) SI_UNIT ( $, .STERADIAN. ) SOLID_ANGLE_UNIT ( ) );
#14957 = VECTOR ( 'NONE', #6670, 1000.000000000000000 ) ;
#14958 = ORIENTED_EDGE ( 'NONE', *, *, #5075, .F. ) ;
#14959 = LINE ( 'NONE', #5952, #11581 ) ;
#14960 = EDGE_CURVE ( 'NONE', #15873, #8683, #3390, .T. ) ;
#14961 = CARTESIAN_POINT ( 'NONE',  ( 49.97728705011488159, 47.49948385550240459, -7.000000000000000888 ) ) ;
#14962 = AXIS2_PLACEMENT_3D ( 'NONE', #6967, #13046, #12755 ) ;
#14963 = EDGE_LOOP ( 'NONE', ( #1246, #15761, #1728, #3038 ) ) ;
#14964 = ORIENTED_EDGE ( 'NONE', *, *, #422, .F. ) ;
#14965 = CARTESIAN_POINT ( 'NONE',  ( 45.31609314410967926, 48.69948385550241454, 6.485486291978119766 ) ) ;
#14966 = LINE ( 'NONE', #166, #6635 ) ;
#14967 = CARTESIAN_POINT ( 'NONE',  ( 47.74827507625478518, 58.59948385550238470, 7.007379884777227730 ) ) ;
#14968 = DIRECTION ( 'NONE',  ( -0.9999670257950099561, -0.008120795692649453515, 0.000000000000000000 ) ) ;
#14969 = CARTESIAN_POINT ( 'NONE',  ( 44.03140696652198471, 51.80051614449766362, 4.306917132069485454 ) ) ;
#14970 = DIRECTION ( 'NONE',  ( 0.000000000000000000, 0.000000000000000000, 1.000000000000000000 ) ) ;
#14971 = CARTESIAN_POINT ( 'NONE',  ( -0.9999999999999976685, -20.00000000000000000, -9.000000000000001776 ) ) ;
#14972 = CARTESIAN_POINT ( 'NONE',  ( 0.000000000000000000, 0.000000000000000000, 0.000000000000000000 ) ) ;
#14973 = ORIENTED_EDGE ( 'NONE', *, *, #10034, .F. ) ;
#14974 = AXIS2_PLACEMENT_3D ( 'NONE', #7046, #4207, #17458 ) ;
#14975 = CIRCLE ( 'NONE', #8078, 5.000000000000000888 ) ;
#14976 = ORIENTED_EDGE ( 'NONE', *, *, #819, .T. ) ;
#14977 = ORIENTED_EDGE ( 'NONE', *, *, #15872, .F. ) ;
#14978 = CARTESIAN_POINT ( 'NONE',  ( -2.100000000000000089, 2.571758278209441957E-16, -4.694516984716113228 ) ) ;
#14979 = MANIFOLD_SOLID_BREP ( 'OuterRace', #524 ) ;
#14980 = CARTESIAN_POINT ( 'NONE',  ( 44.05948171654949874, 46.79948385550238754, 4.345558710429105354 ) ) ;
#14981 = LINE ( 'NONE', #2620, #1518 ) ;
#14982 =( GEOMETRIC_REPRESENTATION_CONTEXT ( 3 ) GLOBAL_UNCERTAINTY_ASSIGNED_CONTEXT ( ( #9482 ) ) GLOBAL_UNIT_ASSIGNED_CONTEXT ( ( #399, #17265, #583 ) ) REPRESENTATION_CONTEXT ( 'NONE', 'WORKASPACE' ) );
#14983 = VERTEX_POINT ( 'NONE', #1365 ) ;
#14984 = FACE_OUTER_BOUND ( 'NONE', #18431, .T. ) ;
#14985 = EDGE_LOOP ( 'NONE', ( #12867, #7631 ) ) ;
#14986 = CARTESIAN_POINT ( 'NONE',  ( 43.34962307344078880, 58.10051614449766078, -2.184720259617096705 ) ) ;
#14987 = ORIENTED_EDGE ( 'NONE', *, *, #13760, .F. ) ;
#14988 = VECTOR ( 'NONE', #5750, 1000.000000000000000 ) ;
#14989 = VECTOR ( 'NONE', #10941, 999.9999999999998863 ) ;
#14990 = CARTESIAN_POINT ( 'NONE',  ( -9.999999999999996447, 25.00000000000001776, -15.00000000000000000 ) ) ;
#14991 = PRODUCT_DEFINITION_CONTEXT ( 'detailed design', #16692, 'design' ) ;
#14992 = CARTESIAN_POINT ( 'NONE',  ( 4.086376042167606748, -1.979461949354202499, 3.571471332069183990 ) ) ;
#14993 = CARTESIAN_POINT ( 'NONE',  ( 55.08986747509849380, 55.20051614449766220, 3.727524721679155384 ) ) ;
#14994 = CARTESIAN_POINT ( 'NONE',  ( 19.89043790736549155, -22.09056926535286891, -9.000000000000000000 ) ) ;
#14995 = DIRECTION ( 'NONE',  ( 0.000000000000000000, 0.000000000000000000, 1.000000000000000000 ) ) ;
#14996 = CARTESIAN_POINT ( 'NONE',  ( 46.45491332379572924, 55.29948385550240175, -4.840751629271157874 ) ) ;
#14997 = COLOUR_RGB ( '',1.000000000000000000, 0.9490196078431372140, 0.9098039215686274384 ) ;
#14998 = CARTESIAN_POINT ( 'NONE',  ( -72.99999999999997158, -1.000000000000000000, 6.000000000000001776 ) ) ;
#14999 = CARTESIAN_POINT ( 'NONE',  ( 52.62207051974829852, 52.60051614449765367, -7.992620115222797139 ) ) ;
#15000 = CARTESIAN_POINT ( 'NONE',  ( 6.212068001624178493, -5.350125758160219291, 0.7333103599835463227 ) ) ;
#15001 = DIRECTION ( 'NONE',  ( -1.000000000000000000, 0.000000000000000000, 0.000000000000000000 ) ) ;
#15002 = EDGE_LOOP ( 'NONE', ( #8371, #10952, #18711, #14934 ) ) ;
#15003 = DIRECTION ( 'NONE',  ( 0.000000000000000000, 0.000000000000000000, -1.000000000000000000 ) ) ;
#15004 =( NAMED_UNIT ( * ) PLANE_ANGLE_UNIT ( ) SI_UNIT ( $, .RADIAN. ) );
#15005 = TOROIDAL_SURFACE ( 'NONE', #18787, 5.899999999999999467, 0.1000000000000010186 ) ;
#15006 = EDGE_CURVE ( 'NONE', #11790, #1052, #2787, .T. ) ;
#15007 = AXIS2_PLACEMENT_3D ( 'NONE', #13072, #2613, #10028 ) ;
#15008 = ORIENTED_EDGE ( 'NONE', *, *, #18751, .F. ) ;
#15009 = DIRECTION ( 'NONE',  ( -0.000000000000000000, -0.000000000000000000, -1.000000000000000000 ) ) ;
#15010 = B_SPLINE_CURVE_WITH_KNOTS ( 'NONE', 3,
 ( #7531, #16371, #3033, #91 ),
 .UNSPECIFIED., .F., .F.,
 ( 4, 4 ),
 ( 2.380735203086575858E-07, 0.002921158011986710323 ),
 .UNSPECIFIED. ) ;
#15011 = DIRECTION ( 'NONE',  ( -9.710251638871371392E-17, -5.969973981896233748E-17, -1.000000000000000000 ) ) ;
#15012 = AXIS2_PLACEMENT_3D ( 'NONE', #18956, #18861, #11373 ) ;
#15013 = CARTESIAN_POINT ( 'NONE',  ( 9.037824375505676855, -37.84146099840244659, 9.000000000000000000 ) ) ;
#15014 = LINE ( 'NONE', #16499, #16510 ) ;
#15015 = AXIS2_PLACEMENT_3D ( 'NONE', #7172, #10195, #19166 ) ;
#15016 = DIRECTION ( 'NONE',  ( 0.000000000000000000, 0.000000000000000000, 1.000000000000000000 ) ) ;
#15017 = VECTOR ( 'NONE', #10778, 1000.000000000000000 ) ;
#15018 = CARTESIAN_POINT ( 'NONE',  ( -54.99999999999996447, -14.99999999999998579, -15.00000000000000000 ) ) ;
#15019 = CARTESIAN_POINT ( 'NONE',  ( 55.96859303347804371, 58.19948385550241454, 4.306917132069425946 ) ) ;
#15020 = EDGE_CURVE ( 'NONE', #12225, #2713, #15088, .T. ) ;
#15021 = DIRECTION ( 'NONE',  ( -1.000000000000000000, 0.000000000000000000, 0.000000000000000000 ) ) ;
#15022 = CARTESIAN_POINT ( 'NONE',  ( 42.38452918213188525, 53.09948385550240602, -2.450534656007040013 ) ) ;
#15023 = CARTESIAN_POINT ( 'NONE',  ( 4.055492966679490330, -2.385006769472456156, -3.005124364834284023 ) ) ;
#15024 = CARTESIAN_POINT ( 'NONE',  ( 45.86712807150329496, 53.70051614449766220, 5.649768623646139964 ) ) ;
#15025 = VECTOR ( 'NONE', #7554, 1000.000000000000000 ) ;
#15026 = CARTESIAN_POINT ( 'NONE',  ( 53.50000000000000000, 0.000000000000000000, 0.000000000000000000 ) ) ;
#15028 = ORIENTED_EDGE ( 'NONE', *, *, #2586, .F. ) ;
#15027 = ADVANCED_FACE ( 'NONE', ( #4598 ), #8998, .T. ) ;
#15029 = EDGE_CURVE ( 'NONE', #402, #4701, #4405, .T. ) ;
#15030 = SURFACE_STYLE_FILL_AREA ( #8589 ) ;
#15031 = ORIENTED_EDGE ( 'NONE', *, *, #18929, .F. ) ;
#15032 = DIRECTION ( 'NONE',  ( 1.000000000000000000, -0.000000000000000000, -0.000000000000000000 ) ) ;
#15033 = VECTOR ( 'NONE', #8075, 1000.000000000000000 ) ;
#15034 = VERTEX_POINT ( 'NONE', #7628 ) ;
#15035 = CARTESIAN_POINT ( 'NONE',  ( -62.49999999999997158, 32.50000000000001421, -9.999999999999998224 ) ) ;
#15036 = EDGE_CURVE ( 'NONE', #6422, #5263, #14981, .T. ) ;
#15037 = CARTESIAN_POINT ( 'NONE',  ( 55.94051828345050836, 61.79948385550239465, -4.345558710429104465 ) ) ;
#15038 = AXIS2_PLACEMENT_3D ( 'NONE', #8462, #1113, #15923 ) ;
#15039 = DIRECTION ( 'NONE',  ( -0.9989677110047504582, -0.04542589977017007230, 1.386346192018204258E-14 ) ) ;
#15040 = EDGE_LOOP ( 'NONE', ( #12389, #1166, #15156, #15957 ) ) ;
#15041 = CARTESIAN_POINT ( 'NONE',  ( -4.158233816355060064, -39.56295201467614220, -9.000000000000000000 ) ) ;
#15042 = DIRECTION ( 'NONE',  ( -1.000000000000000000, 0.000000000000000000, 0.000000000000000000 ) ) ;
#15043 = CARTESIAN_POINT ( 'NONE',  ( 44.88205777487398507, 57.19948385550241454, -3.688883143319540814 ) ) ;
#15044 = EDGE_CURVE ( 'NONE', #8262, #14289, #8902, .T. ) ;
#15045 = DIRECTION ( 'NONE',  ( 2.191393683118470056E-17, 7.538405132783724027E-17, 1.000000000000000000 ) ) ;
#15046 = CARTESIAN_POINT ( 'NONE',  ( 0.4465819873852006072, 2.886751345948123770, -5.000000000000000000 ) ) ;
#15047 = CARTESIAN_POINT ( 'NONE',  ( 56.81924384183006538, 52.80051614449766362, -4.924951120819380357 ) ) ;
#15048 = AXIS2_PLACEMENT_3D ( 'NONE', #10472, #13527, #2947 ) ;
#15049 = CARTESIAN_POINT ( 'NONE',  ( 44.28664221472221385, 55.90051614449766504, 1.832500667257213722 ) ) ;
#15051 = VECTOR ( 'NONE', #16167, 1000.000000000000114 ) ;
#15050 = DIRECTION ( 'NONE',  ( -1.000000000000000000, 0.000000000000000000, 0.000000000000000000 ) ) ;
#15052 = CIRCLE ( 'NONE', #13798, 2.000000000000000000 ) ;
#15053 = CARTESIAN_POINT ( 'NONE',  ( -154.9999999999999716, -6.999999999999993783, 15.00000000000000000 ) ) ;
#15054 = ORIENTED_EDGE ( 'NONE', *, *, #3404, .F. ) ;
#15055 = EDGE_CURVE ( 'NONE', #19390, #153, #12458, .T. ) ;
#15056 = VECTOR ( 'NONE', #17180, 1000.000000000000000 ) ;
#15057 = ORIENTED_EDGE ( 'NONE', *, *, #14240, .F. ) ;
#15058 = CARTESIAN_POINT ( 'NONE',  ( 6.204471256525345702, -0.9979289516723606202, -5.000000000000889955 ) ) ;
#15059 = ORIENTED_EDGE ( 'NONE', *, *, #9511, .F. ) ;
#15060 = CARTESIAN_POINT ( 'NONE',  ( 47.74827507625478518, 62.59948385550240602, 7.007379884777227730 ) ) ;
#15061 = CARTESIAN_POINT ( 'NONE',  ( -13.86289650954791064, -6.617387872822862782, -9.000000000000000000 ) ) ;
#15062 = ORIENTED_EDGE ( 'NONE', *, *, #9844, .T. ) ;
#15063 = DIRECTION ( 'NONE',  ( -1.000000000000000000, 0.000000000000000000, 0.000000000000000000 ) ) ;
#15064 = AXIS2_PLACEMENT_3D ( 'NONE', #9777, #8012, #474 ) ;
#15065 = CARTESIAN_POINT ( 'NONE',  ( 43.33558569842703179, 49.09948385550240602, -2.141517661632099223 ) ) ;
#15066 = ORIENTED_EDGE ( 'NONE', *, *, #1670, .F. ) ;
#15067 = DIRECTION ( 'NONE',  ( 1.000000000000000000, 0.000000000000000000, 0.000000000000000000 ) ) ;
#15068 = CIRCLE ( 'NONE', #2878, 2.000000000000000000 ) ;
#15069 = ORIENTED_EDGE ( 'NONE', *, *, #17915, .F. ) ;
#15070 = CARTESIAN_POINT ( 'NONE',  ( 57.61547081786812896, 48.09948385550240602, 2.450534656007040901 ) ) ;
#15071 = AXIS2_PLACEMENT_3D ( 'NONE', #11199, #5324, #18880 ) ;
#15072 = FACE_OUTER_BOUND ( 'NONE', #7514, .T. ) ;
#15073 = CARTESIAN_POINT ( 'NONE',  ( 54.09612160359786515, 55.69948385550240744, -5.676469297603166098 ) ) ;
#15074 = CARTESIAN_POINT ( 'NONE',  ( 2.354826896168714434, -6.962563485461402024, 0.000000000000000000 ) ) ;
#15075 = CARTESIAN_POINT ( 'NONE',  ( 4.175813232069150338, -4.122719923832746325, 2.362127131240695889E-16 ) ) ;
#15076 = CARTESIAN_POINT ( 'NONE',  ( 54.13287192849671214, 54.70051614449766220, -5.649768623646139964 ) ) ;
#15077 = DIRECTION ( 'NONE',  ( 1.000000000000000000, 1.387778780781445676E-16, 0.000000000000000000 ) ) ;
#15078 = ADVANCED_FACE ( 'NONE', ( #13520 ), #17494, .T. ) ;
#15079 = DIRECTION ( 'NONE',  ( -1.000000000000000000, 0.000000000000000000, 0.000000000000000000 ) ) ;
#15080 = ORIENTED_EDGE ( 'NONE', *, *, #783, .T. ) ;
#15081 = EDGE_CURVE ( 'NONE', #10132, #16421, #6073, .T. ) ;
#15082 = AXIS2_PLACEMENT_3D ( 'NONE', #6709, #10828, #18311 ) ;
#15083 = ORIENTED_EDGE ( 'NONE', *, *, #18323, .T. ) ;
#15084 = ORIENTED_EDGE ( 'NONE', *, *, #6393, .F. ) ;
#15085 = LINE ( 'NONE', #2937, #14019 ) ;
#15086 = CARTESIAN_POINT ( 'NONE',  ( 58.41169779390614281, 63.99948385550241170, -0.02388180880523160798 ) ) ;
#15087 = AXIS2_PLACEMENT_3D ( 'NONE', #7808, #12315, #2034 ) ;
#15088 = LINE ( 'NONE', #1274, #9020 ) ;
#15089 = ORIENTED_EDGE ( 'NONE', *, *, #15623, .T. ) ;
#15090 = CARTESIAN_POINT ( 'NONE',  ( -62.49999999999997158, 40.00000000000001421, 9.999999999999998224 ) ) ;
#15091 = B_SPLINE_CURVE_WITH_KNOTS ( 'NONE', 3,
 ( #15840, #13185, #14357, #10231, #2529 ),
 .UNSPECIFIED., .F., .F.,
 ( 4, 1, 4 ),
 ( 9.359404341228126911E-20, 0.002886751345948132021, 0.005773502691896264041 ),
 .UNSPECIFIED. ) ;
#15092 = EDGE_LOOP ( 'NONE', ( #18356, #11818, #4580, #7419 ) ) ;
#15093 = CARTESIAN_POINT ( 'NONE',  ( 52.29715082351539479, 60.60051614449764656, -6.992620115222796251 ) ) ;
#15094 = ORIENTED_EDGE ( 'NONE', *, *, #1978, .F. ) ;
#15095 = CARTESIAN_POINT ( 'NONE',  ( 0.6448876103708359731, 4.246476118072354922, -0.2256878752776725616 ) ) ;
#15096 = B_SPLINE_CURVE_WITH_KNOTS ( 'NONE', 3,
 ( #13065, #5615, #1208, #1021, #2786, #8748 ),
 .UNSPECIFIED., .F., .F.,
 ( 4, 2, 4 ),
 ( -3.640115492410698714E-06, 0.0002066546034006521879, 0.0004169493222937151081 ),
 .UNSPECIFIED. ) ;
#15097 = CARTESIAN_POINT ( 'NONE',  ( -0.9996874511566050669, -39.97499999999999432, -9.000000000000000000 ) ) ;
#15098 = CARTESIAN_POINT ( 'NONE',  ( 49.97728705011494554, 55.50051614449766646, 6.000000000000000888 ) ) ;
#15099 = CARTESIAN_POINT ( 'NONE',  ( 8.673617379884035472E-16, 4.618802153517012954, -5.000000000000000000 ) ) ;
#15100 = ADVANCED_FACE ( 'NONE', ( #6159 ), #10559, .T. ) ;
#15101 = VECTOR ( 'NONE', #5959, 1000.000000000000000 ) ;
#15102 = CARTESIAN_POINT ( 'NONE',  ( 48.07319477248768180, 58.59948385550239891, 6.007379884777225953 ) ) ;
#15103 = CARTESIAN_POINT ( 'NONE',  ( -0.1750025118121544265, -4.719839900820635314, -3.469254087858253399 ) ) ;
#15104 = CARTESIAN_POINT ( 'NONE',  ( 41.58830220609386430, 54.00051614449765935, -0.02388180880514929535 ) ) ;
#15105 = CARTESIAN_POINT ( 'NONE',  ( -65.14999999999996305, 32.50000000000001421, 15.00000000000000000 ) ) ;
#15106 = CARTESIAN_POINT ( 'NONE',  ( 4.055492966679587141, 3.795017426214561063, -0.5629142681441071661 ) ) ;
#15107 = ORIENTED_EDGE ( 'NONE', *, *, #13270, .F. ) ;
#15108 = CARTESIAN_POINT ( 'NONE',  ( 0.000000000000000000, 0.000000000000000000, 0.000000000000000000 ) ) ;
#15109 = APPLICATION_PROTOCOL_DEFINITION ( 'draft international standard', 'automotive_design', 1998, #7655 ) ;
#15110 = VECTOR ( 'NONE', #5833, 1000.000000000000000 ) ;
#15111 = ORIENTED_EDGE ( 'NONE', *, *, #9442, .F. ) ;
#15112 = DIRECTION ( 'NONE',  ( -0.000000000000000000, 0.000000000000000000, 1.000000000000000000 ) ) ;
#15113 = FACE_OUTER_BOUND ( 'NONE', #4260, .T. ) ;
#15114 = CARTESIAN_POINT ( 'NONE',  ( 4.000000000000000000, 0.000000000000000000, 0.000000000000000000 ) ) ;
#15115 = CARTESIAN_POINT ( 'NONE',  ( 6.495567275915077765, 2.917443832164883233, 5.053160945538031079 ) ) ;
#15116 = DIRECTION ( 'NONE',  ( -0.000000000000000000, -0.000000000000000000, 1.000000000000000000 ) ) ;
#15117 = CARTESIAN_POINT ( 'NONE',  ( 4.200000000000001954, 0.000000000000000000, 0.000000000000000000 ) ) ;
#15118 = CARTESIAN_POINT ( 'NONE',  ( 43.33558569842703179, 59.09948385550240602, -2.141517661632099223 ) ) ;
#15119 = CARTESIAN_POINT ( 'NONE',  ( -57.64999999999994884, -14.99999999999998579, 10.00000000000000000 ) ) ;
#15120 = CARTESIAN_POINT ( 'NONE',  ( 47.37792948025162332, 51.39948385550241028, -7.992620115222770494 ) ) ;
#15121 = DIRECTION ( 'NONE',  ( 0.000000000000000000, 0.000000000000000000, 1.000000000000000000 ) ) ;
#15122 = CARTESIAN_POINT ( 'NONE',  ( 44.05948171654945611, 52.20051614449764799, -4.345558710429044069 ) ) ;
#15123 = DIRECTION ( 'NONE',  ( 1.000000000000000000, 0.000000000000000000, 0.000000000000000000 ) ) ;
#15124 = SHAPE_REPRESENTATION_RELATIONSHIP ( 'NONE' , 'NONE' ,  #18081, #8234 ) ;
#15125 = VERTEX_POINT ( 'NONE', #16564 ) ;
#15126 = DIRECTION ( 'NONE',  ( 1.000000000000000000, 0.000000000000000000, 0.000000000000000000 ) ) ;
#15127 = ORIENTED_EDGE ( 'NONE', *, *, #18171, .T. ) ;
#15128 = CARTESIAN_POINT ( 'NONE',  ( 2.482347295856823136E-15, -20.00000000000000000, -8.999999999999996447 ) ) ;
#15129 = CARTESIAN_POINT ( 'NONE',  ( 44.03140696652192787, 65.19948385550240744, -4.306917132069425058 ) ) ;
#15130 = CARTESIAN_POINT ( 'NONE',  ( -0.1481481481481481122, -4.797713218419819903, 0.000000000000000000 ) ) ;
#15131 = EDGE_LOOP ( 'NONE', ( #15726, #19316, #2985, #3120, #1637 ) ) ;
#15132 = LINE ( 'NONE', #139, #6462 ) ;
#15133 = CYLINDRICAL_SURFACE ( 'NONE', #18295, 4.000000000000000000 ) ;
#15134 = EDGE_CURVE ( 'NONE', #6607, #7017, #11521, .T. ) ;
#15135 = CARTESIAN_POINT ( 'NONE',  ( 44.30067958973596376, 54.89948385550240317, 1.875703265242204099 ) ) ;
#15136 = CARTESIAN_POINT ( 'NONE',  ( -74.99999999999997158, 40.00000000000001421, 15.00000000000000000 ) ) ;
#15137 = CARTESIAN_POINT ( 'NONE',  ( -159.0000000000000000, -14.99999999999999645, -15.79999999999999538 ) ) ;
#15138 = CARTESIAN_POINT ( 'NONE',  ( 52.62207051974829852, 54.60051614449766788, -7.992620115222797139 ) ) ;
#15139 = CARTESIAN_POINT ( 'NONE',  ( 50.02271294988506156, 54.50051614449765935, -6.000000000000000888 ) ) ;
#15140 = EDGE_CURVE ( 'NONE', #11712, #12595, #7338, .T. ) ;
#15141 = DIRECTION ( 'NONE',  ( 1.000000000000000000, 0.000000000000000000, 0.000000000000000000 ) ) ;
#15142 = CARTESIAN_POINT ( 'NONE',  ( 6.092449800118536096, -4.833012432206597708, -1.628976913806147397 ) ) ;
#15143 = VERTEX_POINT ( 'NONE', #11840 ) ;
#15144 = EDGE_CURVE ( 'NONE', #4647, #11260, #9334, .T. ) ;
#15145 = EDGE_CURVE ( 'NONE', #18302, #15442, #8814, .T. ) ;
#15146 = VERTEX_POINT ( 'NONE', #13701 ) ;
#15147 = CARTESIAN_POINT ( 'NONE',  ( 6.541333988313477121, -2.987057409892287740, -5.112749828287758369 ) ) ;
#15148 = ORIENTED_EDGE ( 'NONE', *, *, #5317, .T. ) ;
#15149 = EDGE_CURVE ( 'NONE', #19012, #660, #6850, .T. ) ;
#15150 = DIRECTION ( 'NONE',  ( 1.000000000000000000, -0.000000000000000000, -0.000000000000000000 ) ) ;
#15151 = CARTESIAN_POINT ( 'NONE',  ( -74.99999999999997158, 32.50000000000001421, 15.00000000000000000 ) ) ;
#15152 = ORIENTED_EDGE ( 'NONE', *, *, #5802, .F. ) ;
#15153 = DIRECTION ( 'NONE',  ( 0.000000000000000000, 0.000000000000000000, 1.000000000000000000 ) ) ;
#15154 = CARTESIAN_POINT ( 'NONE',  ( 52.29715082351547295, 50.39948385550241028, 6.992620115222774047 ) ) ;
#15155 = VECTOR ( 'NONE', #339, 1000.000000000000000 ) ;
#15156 = ORIENTED_EDGE ( 'NONE', *, *, #6281, .T. ) ;
#15157 = FACE_OUTER_BOUND ( 'NONE', #13357, .T. ) ;
#15158 = ORIENTED_EDGE ( 'NONE', *, *, #752, .F. ) ;
#15159 = CARTESIAN_POINT ( 'NONE',  ( 57.61547081786812896, 46.09948385550240602, 2.450534656007040901 ) ) ;
#15160 = VECTOR ( 'NONE', #18075, 1000.000000000000227 ) ;
#15161 = DIRECTION ( 'NONE',  ( -9.710251638871371392E-17, -5.969973981896233748E-17, -1.000000000000000000 ) ) ;
#15162 = EDGE_CURVE ( 'NONE', #10053, #8597, #13423, .T. ) ;
#15163 = CARTESIAN_POINT ( 'NONE',  ( 47.70284917648453415, 57.39948385550241028, -6.992620115222774047 ) ) ;
#15164 = DIRECTION ( 'NONE',  ( 0.000000000000000000, 1.000000000000000000, 0.000000000000000000 ) ) ;
#15165 = ADVANCED_FACE ( 'NONE', ( #18528 ), #2042, .F. ) ;
#15166 = CARTESIAN_POINT ( 'NONE',  ( 4.000000000000000000, -1.942223658245635809, -0.3516579909967643691 ) ) ;
#15167 = CARTESIAN_POINT ( 'NONE',  ( 52.29715082351538769, 56.60051614449766788, -6.992620115222796251 ) ) ;
#15168 = CARTESIAN_POINT ( 'NONE',  ( 6.196878017913833858, -1.924500897298759172, -5.000000000000000888 ) ) ;
#15169 = CARTESIAN_POINT ( 'NONE',  ( -18.02113032590304442, -26.18033988749903074, -9.000000000000000000 ) ) ;
#15170 = ORIENTED_EDGE ( 'NONE', *, *, #18537, .T. ) ;
#15171 = ORIENTED_EDGE ( 'NONE', *, *, #11970, .T. ) ;
#15172 = EDGE_LOOP ( 'NONE', ( #13370, #5186, #7088, #11968 ) ) ;
#15173 = DIRECTION ( 'NONE',  ( -1.000000000000000000, -0.000000000000000000, -0.000000000000000000 ) ) ;
#15174 = AXIS2_PLACEMENT_3D ( 'NONE', #15793, #992, #5487 ) ;
#15175 = CARTESIAN_POINT ( 'NONE',  ( 42.39856655714566358, 64.89948385550239607, 2.493737253992119207 ) ) ;
#15176 = DIRECTION ( 'NONE',  ( -0.9768494444668812671, -0.2139279384389642935, 0.000000000000000000 ) ) ;
#15177 = ORIENTED_EDGE ( 'NONE', *, *, #17189, .F. ) ;
#15178 = DIRECTION ( 'NONE',  ( 1.000000000000000000, 0.000000000000000000, 0.000000000000000000 ) ) ;
#15179 = ORIENTED_EDGE ( 'NONE', *, *, #15270, .T. ) ;
#15180 = CARTESIAN_POINT ( 'NONE',  ( 45.90387839640208512, 60.30051614449766362, -5.676469297603124353 ) ) ;
#15181 = VERTEX_POINT ( 'NONE', #4970 ) ;
#15182 = CARTESIAN_POINT ( 'NONE',  ( 0.000000000000000000, 0.000000000000000000, -25.03750572909317285 ) ) ;
#15183 = UNCERTAINTY_MEASURE_WITH_UNIT (LENGTH_MEASURE( 1.000000000000000082E-05 ), #17088, 'distance_accuracy_value', 'NONE');
#15184 = LINE ( 'NONE', #3427, #16514 ) ;
#15185 = VECTOR ( 'NONE', #7940, 1000.000000000000000 ) ;
#15186 = AXIS2_PLACEMENT_3D ( 'NONE', #18727, #5465, #9781 ) ;
#15187 = CARTESIAN_POINT ( 'NONE',  ( 53.50833635130544508, 57.30051614449767072, 4.867452303228181343 ) ) ;
#15188 = CARTESIAN_POINT ( 'NONE',  ( 0.3106000600989267113, 3.122278952918445150, -4.592054218142293642 ) ) ;
#15189 = DIRECTION ( 'NONE',  ( 0.000000000000000000, 0.000000000000000000, 1.000000000000000000 ) ) ;
#15190 = EDGE_CURVE ( 'NONE', #10087, #1056, #10661, .T. ) ;
#15191 = CARTESIAN_POINT ( 'NONE',  ( 55.71335778527780747, 60.09948385550240602, 1.832500667257165983 ) ) ;
#15192 = CARTESIAN_POINT ( 'NONE',  ( -2.500000000000000444, 3.061616997868383634E-16, -25.03750572909317285 ) ) ;
#15193 = CARTESIAN_POINT ( 'NONE',  ( 47.42335538002180328, 54.40051614449765793, -8.007379884777206414 ) ) ;
#15194 = DIRECTION ( 'NONE',  ( -0.000000000000000000, -0.000000000000000000, 1.000000000000000000 ) ) ;
#15195 = ORIENTED_EDGE ( 'NONE', *, *, #10705, .F. ) ;
#15196 = DIRECTION ( 'NONE',  ( 1.000000000000000000, -6.938893903907227392E-16, 0.000000000000000000 ) ) ;
#15197 =( NAMED_UNIT ( * ) PLANE_ANGLE_UNIT ( ) SI_UNIT ( $, .RADIAN. ) );
#15198 = DIRECTION ( 'NONE',  ( 1.000000000000000000, 0.000000000000000000, 0.000000000000000000 ) ) ;
#15199 = SHAPE_DEFINITION_REPRESENTATION ( #9750, #4676 ) ;
#15200 = EDGE_LOOP ( 'NONE', ( #3527, #9004 ) ) ;
#15201 = CARTESIAN_POINT ( 'NONE',  ( 1.149999999999998135, 0.000000000000000000, 0.000000000000000000 ) ) ;
#15202 = ADVANCED_FACE ( 'NONE', ( #12232 ), #5908, .F. ) ;
#15203 = DIRECTION ( 'NONE',  ( 0.000000000000000000, 0.000000000000000000, 1.000000000000000000 ) ) ;
#15204 = AXIS2_PLACEMENT_3D ( 'NONE', #5777, #17748, #5681 ) ;
#15205 = EDGE_CURVE ( 'NONE', #11016, #11915, #6350, .T. ) ;
#15206 = MANIFOLD_SOLID_BREP ( 'M4 Clearance Hole1', #3050 ) ;
#15207 = CARTESIAN_POINT ( 'NONE',  ( 45.90387839640214196, 64.69948385550240744, 5.676469297603166098 ) ) ;
#15208 = CYLINDRICAL_SURFACE ( 'NONE', #10228, 3.799999999999999378 ) ;
#15209 = LINE ( 'NONE', #5105, #13898 ) ;
#15210 = CARTESIAN_POINT ( 'NONE',  ( 17.79870116617236420, -10.87825472854593478, 0.000000000000000000 ) ) ;
#15211 = COLOUR_RGB ( '',1.000000000000000000, 0.9490196078431372140, 0.9098039215686274384 ) ;
#15212 = CARTESIAN_POINT ( 'NONE',  ( 54.09612160359786515, 59.69948385550240033, -5.676469297603166098 ) ) ;
#15213 = DIRECTION ( 'NONE',  ( 1.000000000000000000, 0.000000000000000000, 0.000000000000000000 ) ) ;
#15214 = CARTESIAN_POINT ( 'NONE',  ( 43.20883090819745576, 60.79948385550241596, 4.963592699179006473 ) ) ;
#15215 = CARTESIAN_POINT ( 'NONE',  ( 44.05948171654945611, 56.20051614449764799, -4.345558710429044069 ) ) ;
#15216 = CARTESIAN_POINT ( 'NONE',  ( -74.99999999999997158, 40.00000000000001421, -4.999999999999984013 ) ) ;
#15217 = CARTESIAN_POINT ( 'NONE',  ( 49.99999999999997158, 45.00000000000001421, -7.000000000000000888 ) ) ;
#15218 = AXIS2_PLACEMENT_3D ( 'NONE', #2545, #19215, #11526 ) ;
#15219 = ORIENTED_EDGE ( 'NONE', *, *, #17077, .F. ) ;
#15220 =( GEOMETRIC_REPRESENTATION_CONTEXT ( 3 ) GLOBAL_UNCERTAINTY_ASSIGNED_CONTEXT ( ( #7939 ) ) GLOBAL_UNIT_ASSIGNED_CONTEXT ( ( #13431, #4216, #11957 ) ) REPRESENTATION_CONTEXT ( 'NONE', 'WORKASPACE' ) );
#15221 = CARTESIAN_POINT ( 'NONE',  ( 0.1381419387168661417, -1.355287006802423644, -3.499999999999999556 ) ) ;
#15222 = CARTESIAN_POINT ( 'NONE',  ( 54.09612160359792199, 45.30051614449766362, 5.676469297603124353 ) ) ;
#15223 = DIRECTION ( 'NONE',  ( 0.000000000000000000, 0.000000000000000000, 1.000000000000000000 ) ) ;
#15224 = CARTESIAN_POINT ( 'NONE',  ( 18.00000000000000355, -20.00000000000000000, -20.00000000000000000 ) ) ;
#15225 = ORIENTED_EDGE ( 'NONE', *, *, #3544, .T. ) ;
#15226 = CARTESIAN_POINT ( 'NONE',  ( 5.599999999999998757, 6.472876824008161592E-16, -5.200000000000001066 ) ) ;
#15227 = AXIS2_PLACEMENT_3D ( 'NONE', #13321, #16282, #19340 ) ;
#15228 = CARTESIAN_POINT ( 'NONE',  ( -10.93224627749298783, -36.74771600333134103, 9.000000000000000000 ) ) ;
#15229 = CARTESIAN_POINT ( 'NONE',  ( 44.88205777487398507, 65.19948385550240744, -3.688883143319540814 ) ) ;
#15230 = DIRECTION ( 'NONE',  ( 0.000000000000000000, -0.000000000000000000, 1.000000000000000000 ) ) ;
#15231 = DIRECTION ( 'NONE',  ( 1.000000000000000000, 0.000000000000000000, 0.000000000000000000 ) ) ;
#15232 = CARTESIAN_POINT ( 'NONE',  ( 42.39856655714564226, 52.10051614449766788, -2.493737253992044156 ) ) ;
#15233 = CARTESIAN_POINT ( 'NONE',  ( 50.02271294988506156, 52.50051614449766646, -6.000000000000000888 ) ) ;
#15234 = CARTESIAN_POINT ( 'NONE',  ( 1.393927851585479161, -4.043713361053543842, -3.526374918436840922 ) ) ;
#15235 = CARTESIAN_POINT ( 'NONE',  ( 6.242800618755285136, -4.918813924287352535, -1.690830708135802052 ) ) ;
#15236 = EDGE_LOOP ( 'NONE', ( #16737, #7433, #15691 ) ) ;
#15237 = AXIS2_PLACEMENT_3D ( 'NONE', #6029, #6118, #14937 ) ;
#15238 = ORIENTED_EDGE ( 'NONE', *, *, #3944, .F. ) ;
#15239 = CARTESIAN_POINT ( 'NONE',  ( -20.63749999999999574, 0.000000000000000000, 0.000000000000000000 ) ) ;
#15240 = VECTOR ( 'NONE', #11828, 1000.000000000000000 ) ;
#15241 = ORIENTED_EDGE ( 'NONE', *, *, #1392, .F. ) ;
#15242 = ADVANCED_FACE ( 'NONE', ( #11040 ), #6533, .T. ) ;
#15243 = CARTESIAN_POINT ( 'NONE',  ( -155.0818120241833640, -18.99916326157099533, 15.00000000000000000 ) ) ;
#15244 = ORIENTED_EDGE ( 'NONE', *, *, #5001, .T. ) ;
#15245 = PLANE ( 'NONE',  #4084 ) ;
#15246 = CARTESIAN_POINT ( 'NONE',  ( 54.09612160359786515, 53.69948385550240744, -5.676469297603166098 ) ) ;
#15247 = ORIENTED_EDGE ( 'NONE', *, *, #15386, .F. ) ;
#15248 = DIRECTION ( 'NONE',  ( 0.000000000000000000, 0.000000000000000000, -1.000000000000000000 ) ) ;
#15249 = VERTEX_POINT ( 'NONE', #3512 ) ;
#15250 = CARTESIAN_POINT ( 'NONE',  ( 57.60143344285435774, 63.10051614449766078, 2.493737253992045044 ) ) ;
#15251 = DIRECTION ( 'NONE',  ( 0.000000000000000000, 0.000000000000000000, 1.000000000000000000 ) ) ;
#15252 = AXIS2_PLACEMENT_3D ( 'NONE', #13025, #2462, #15976 ) ;
#15253 = CARTESIAN_POINT ( 'NONE',  ( 48.07319477248768180, 46.59948385550239891, 6.007379884777225953 ) ) ;
#15254 = LINE ( 'NONE', #16654, #13677 ) ;
#15255 = CARTESIAN_POINT ( 'NONE',  ( 3.999999999999999112, -0.7890432684750902093, -0.04868663549882291247 ) ) ;
#15256 = ADVANCED_BREP_SHAPE_REPRESENTATION ( '', ( #8790, #10359 ), #11203 ) ;
#15257 = CARTESIAN_POINT ( 'NONE',  ( 43.34962307344078880, 52.10051614449766078, -2.184720259617096705 ) ) ;
#15258 = ADVANCED_FACE ( 'NONE', ( #15271 ), #12517, .F. ) ;
#15259 = DIRECTION ( 'NONE',  ( 0.000000000000000000, 0.000000000000000000, 1.000000000000000000 ) ) ;
#15260 = ADVANCED_FACE ( 'NONE', ( #4795 ), #17046, .F. ) ;
#15261 = CARTESIAN_POINT ( 'NONE',  ( 44.03140696652192787, 53.19948385550238612, -4.306917132069425058 ) ) ;
#15262 = PLANE ( 'NONE',  #17260 ) ;
#15263 = ORIENTED_EDGE ( 'NONE', *, *, #4008, .F. ) ;
#15264 = VECTOR ( 'NONE', #7179, 1000.000000000000000 ) ;
#15265 = ORIENTED_EDGE ( 'NONE', *, *, #19126, .F. ) ;
#15266 = DIRECTION ( 'NONE',  ( 0.000000000000000000, 0.000000000000000000, 1.000000000000000000 ) ) ;
#15267 = EDGE_CURVE ( 'NONE', #11811, #671, #3322, .T. ) ;
#15268 = AXIS2_PLACEMENT_3D ( 'NONE', #14604, #19160, #11669 ) ;
#15269 = CARTESIAN_POINT ( 'NONE',  ( 44.03140696652192787, 55.19948385550238612, -4.306917132069425058 ) ) ;
#15270 = EDGE_CURVE ( 'NONE', #1555, #19038, #12891, .T. ) ;
#15271 = FACE_OUTER_BOUND ( 'NONE', #2468, .T. ) ;
#15272 = ORIENTED_EDGE ( 'NONE', *, *, #6994, .F. ) ;
#15273 = CIRCLE ( 'NONE', #14321, 4.599999999999999645 ) ;
#15274 = CYLINDRICAL_SURFACE ( 'NONE', #3630, 2.000000000000001776 ) ;
#15275 = ORIENTED_EDGE ( 'NONE', *, *, #16517, .F. ) ;
#15276 = CARTESIAN_POINT ( 'NONE',  ( 47.74827507625470702, 58.40051614449766504, -7.007379884777204637 ) ) ;
#15277 = ORIENTED_EDGE ( 'NONE', *, *, #12208, .T. ) ;
#15278 = ADVANCED_FACE ( 'NONE', ( #9280, #3991 ), #11335, .T. ) ;
#15279 = CARTESIAN_POINT ( 'NONE',  ( -4.999999999999998224, -20.00000000000000000, 15.00000000000000355 ) ) ;
#15280 = B_SPLINE_CURVE_WITH_KNOTS ( 'NONE', 3,
 ( #1641, #7217, #10342, #5749 ),
 .UNSPECIFIED., .F., .F.,
 ( 4, 4 ),
 ( 2.380735200831296902E-07, 0.002921158011986723767 ),
 .UNSPECIFIED. ) ;
#15281 = CARTESIAN_POINT ( 'NONE',  ( -52.34999999999998010, -14.99999999999998579, 10.00000000000000000 ) ) ;
#15282 = EDGE_CURVE ( 'NONE', #6580, #6930, #17141, .T. ) ;
#15283 = CARTESIAN_POINT ( 'NONE',  ( 53.54508667620424234, 52.70051614449766220, -4.840751629271188961 ) ) ;
#15284 = CARTESIAN_POINT ( 'NONE',  ( 0.4465819873852006072, 2.886751345948123770, -5.000000000000000000 ) ) ;
#15285 = AXIS2_PLACEMENT_3D ( 'NONE', #18161, #3251, #9211 ) ;
#15286 = ADVANCED_FACE ( 'NONE', ( #16057 ), #1147, .F. ) ;
#15287 = CARTESIAN_POINT ( 'NONE',  ( 48.02776887271750184, 45.60051614449765367, 5.992620115222795363 ) ) ;
#15288 = DIRECTION ( 'NONE',  ( 1.000000000000000000, 0.000000000000000000, 0.000000000000000000 ) ) ;
#15289 = CARTESIAN_POINT ( 'NONE',  ( 45.27934281921082516, 57.70051614449766930, 6.458785618021089192 ) ) ;
#15290 = STYLED_ITEM ( 'NONE', ( #12732 ), #780 ) ;
#15291 = EDGE_LOOP ( 'NONE', ( #6458, #14498 ) ) ;
#15292 = CARTESIAN_POINT ( 'NONE',  ( 2.449293598294706513E-15, -20.00000000000000000, -8.999999999999998224 ) ) ;
#15293 = ORIENTED_EDGE ( 'NONE', *, *, #15912, .F. ) ;
#15294 = B_SPLINE_CURVE_WITH_KNOTS ( 'NONE', 3,
 ( #4049, #5507, #14227, #3854 ),
 .UNSPECIFIED., .F., .F.,
 ( 4, 4 ),
 ( 2.380735200829041677E-07, 0.002921158011986707288 ),
 .UNSPECIFIED. ) ;
#15295 = FACE_OUTER_BOUND ( 'NONE', #12970, .T. ) ;
#15296 = SHAPE_DEFINITION_REPRESENTATION ( #14778, #13428 ) ;
#15297 = EDGE_LOOP ( 'NONE', ( #16381, #9479, #7673, #2933 ) ) ;
#15298 = LINE ( 'NONE', #13824, #3306 ) ;
#15299 = VECTOR ( 'NONE', #16375, 1000.000000000000114 ) ;
#15300 = VECTOR ( 'NONE', #16342, 1000.000000000000000 ) ;
#15301 = DIRECTION ( 'NONE',  ( -1.000000000000000000, 0.000000000000000000, 0.000000000000000000 ) ) ;
#15302 =( REPRESENTATION_RELATIONSHIP ('NONE','NONE', #16703, #659 ) REPRESENTATION_RELATIONSHIP_WITH_TRANSFORMATION ( #4815 )SHAPE_REPRESENTATION_RELATIONSHIP( ) );
#15303 = CARTESIAN_POINT ( 'NONE',  ( 47.74827507625477807, 62.59948385550239891, 7.007379884777229506 ) ) ;
#15304 = CARTESIAN_POINT ( 'NONE',  ( 3.951447005078451813, 3.704664227300101143, 0.5833333333333334814 ) ) ;
#15305 = DIRECTION ( 'NONE',  ( 0.000000000000000000, 0.000000000000000000, 1.000000000000000000 ) ) ;
#15306 = FACE_OUTER_BOUND ( 'NONE', #18638, .T. ) ;
#15307 = CARTESIAN_POINT ( 'NONE',  ( 51.92680522751233951, 47.59948385550239891, -6.007379884777223289 ) ) ;
#15308 = LINE ( 'NONE', #18566, #12566 ) ;
#15309 = CARTESIAN_POINT ( 'NONE',  ( 58.41169779390614281, 61.99948385550241170, -0.02388180880523160798 ) ) ;
#15310 = CARTESIAN_POINT ( 'NONE',  ( 52.25172492374527877, 57.40051614449765083, 7.007379884777203749 ) ) ;
#15311 = EDGE_CURVE ( 'NONE', #11836, #1321, #13738, .T. ) ;
#15312 = VECTOR ( 'NONE', #1030, 1000.000000000000000 ) ;
#15313 =( BOUNDED_CURVE ( )  B_SPLINE_CURVE ( 2, ( #15511, #3555, #6391, #6483, #13843, #1995, #15222, #17093, #6310, #9232, #3269, #425, #7870, #9522, #16903, #12282, #12369, #1901, #18378, #6586, #18474, #18282, #4835, #1803, #3467, #5024, #14024, #10798, #4925, #9430, #15321, #15414, #16801, #609, #7674, #12570, #7958, #18578, #13928, #7772, #5116, #9330, #13655, #229, #6208, #10710, #12180, #18193, #4751, #16707, #13747, #18867, #12952, #8246, #11183, #8341, #13054, #3747, #12763, #5308, #7071, #14516, #17292, #19064, #5208, #14127, #14322, #15906, #1100, #4411, #15608, #18961, #9809, #5605, #902, #6974, #6779, #5502, #8445, #12665, #16010, #11575, #6872, #11475, #2188, #17485, #18668, #18763, #11283, #17188, #8152, #712, #17591, #17385, #4044, #6683, #2491, #2390, #1009, #14221, #9714, #10007, #15713, #2596, #2293, #806, #3849, #15808, #12862, #5405, #11378, #3946, #9906, #14428, #8546, #4705, #10378, #17952, #10667, #9003, #7632, #7726, #11949, #9287, #3142, #13708, #16672, #16380, #12045, #10469, #3039, #3236, #2945, #7822, #14986, #190, #16568, #15276, #3327, #4799, #18143, #1570, #1856, #18045, #13803, #1, #8907, #9106, #9195, #387, #18338, #13612, #283, #12331, #6354, #6166, #15180, #1760, #12239, #15093, #5982, #10762, #12138, #6259, #14887, #1463, #16759, #7443, #7539, #13421, #4512, #16473, #13524, #97, #6077, #4603, #10564, #18245, #1668, #7915, #15374, #12525, #9668, #3707, #18535, #2048, #5268, #3608, #4977, #12718, #14276, #8298, #5078, #472, #672, #14083, #9382, #18721, #6642 ),
 .UNSPECIFIED., .F., .F. ) 
 B_SPLINE_CURVE_WITH_KNOTS ( ( 3, 2, 2, 2, 2, 2, 2, 2, 2, 2, 2, 2, 2, 2, 2, 2, 2, 2, 2, 2, 2, 2, 2, 2, 2, 2, 2, 2, 2, 2, 2, 2, 2, 2, 2, 2, 2, 2, 2, 2, 2, 2, 2, 2, 2, 2, 2, 2, 2, 2, 2, 2, 2, 2, 2, 2, 2, 2, 2, 2, 2, 2, 2, 2, 2, 2, 2, 2, 2, 2, 2, 2, 2, 2, 2, 2, 2, 2, 2, 2, 2, 2, 2, 2, 2, 2, 2, 2, 2, 2, 2, 2, 2, 2, 2, 2, 2, 2, 2, 3 ),
 ( 0.01230184727895902198, 0.02000000000000000042, 0.02999999999999999889, 0.04000000000000000083, 0.05000000000000000278, 0.05999999999999999778, 0.07000000000000000666, 0.08000000000000000167, 0.08999999999999999667, 0.1000000000000000056, 0.1100000000000000006, 0.1199999999999999956, 0.1300000000000000044, 0.1400000000000000133, 0.1499999999999999944, 0.1600000000000000033, 0.1700000000000000122, 0.1799999999999999933, 0.1900000000000000022, 0.2000000000000000111, 0.2099999999999999922, 0.2200000000000000011, 0.2300000000000000100, 0.2399999999999999911, 0.2500000000000000000, 0.2600000000000000089, 0.2700000000000000178, 0.2800000000000000266, 0.2899999999999999800, 0.2999999999999999889, 0.3099999999999999978, 0.3200000000000000067, 0.3300000000000000155, 0.3400000000000000244, 0.3499999999999999778, 0.3599999999999999867, 0.3699999999999999956, 0.3800000000000000044, 0.3900000000000000133, 0.4000000000000000222, 0.4099999999999999756, 0.4199999999999999845, 0.4299999999999999933, 0.4400000000000000022, 0.4500000000000000111, 0.4600000000000000200, 0.4699999999999999734, 0.4799999999999999822, 0.4899999999999999911, 0.5000000000000000000, 0.5100000000000000089, 0.5200000000000000178, 0.5300000000000000266, 0.5400000000000000355, 0.5500000000000000444, 0.5600000000000000533, 0.5699999999999999512, 0.5799999999999999600, 0.5899999999999999689, 0.5999999999999999778, 0.6099999999999999867, 0.6199999999999999956, 0.6300000000000000044, 0.6400000000000000133, 0.6500000000000000222, 0.6600000000000000311, 0.6700000000000000400, 0.6800000000000000488, 0.6899999999999999467, 0.6999999999999999556, 0.7099999999999999645, 0.7199999999999999734, 0.7299999999999999822, 0.7399999999999999911, 0.7500000000000000000, 0.7600000000000000089, 0.7700000000000000178, 0.7800000000000000266, 0.7900000000000000355, 0.8000000000000000444, 0.8100000000000000533, 0.8199999999999999512, 0.8299999999999999600, 0.8399999999999999689, 0.8499999999999999778, 0.8599999999999999867, 0.8699999999999999956, 0.8800000000000000044, 0.8900000000000000133, 0.9000000000000000222, 0.9100000000000000311, 0.9200000000000000400, 0.9300000000000000488, 0.9399999999999999467, 0.9499999999999999556, 0.9599999999999999645, 0.9699999999999999734, 0.9799999999999999822, 0.9899999999999999911, 1.000000000000000000 ),
 .UNSPECIFIED. ) 
 CURVE ( )  GEOMETRIC_REPRESENTATION_ITEM ( )  RATIONAL_B_SPLINE_CURVE ( ( 0.9826544568871729002, 0.9623225587740311671, 1.000000000000000000, 0.9510565162951535312, 1.000000000000000000, 0.9510565162951535312, 1.000000000000000000, 0.9510565162951535312, 1.000000000000000000, 0.9510565162951535312, 1.000000000000000000, 0.9510565162951535312, 1.000000000000000000, 0.9510565162951535312, 1.000000000000000000, 0.9510565162951535312, 1.000000000000000000, 0.9510565162951535312, 1.000000000000000000, 0.9510565162951535312, 1.000000000000000000, 0.9510565162951535312, 1.000000000000000000, 0.9510565162951535312, 1.000000000000000000, 0.9510565162951535312, 1.000000000000000000, 0.9510565162951535312, 1.000000000000000000, 0.9510565162951535312, 1.000000000000000000, 0.9510565162951535312, 1.000000000000000000, 0.9510565162951535312, 1.000000000000000000, 0.9510565162951535312, 1.000000000000000000, 0.9510565162951535312, 1.000000000000000000, 0.9510565162951535312, 1.000000000000000000, 0.9510565162951535312, 1.000000000000000000, 0.9510565162951535312, 1.000000000000000000, 0.9510565162951535312, 1.000000000000000000, 0.9510565162951535312, 1.000000000000000000, 0.9510565162951535312, 1.000000000000000000, 0.9510565162951535312, 1.000000000000000000, 0.9510565162951535312, 1.000000000000000000, 0.9510565162951535312, 1.000000000000000000, 0.9510565162951535312, 1.000000000000000000, 0.9510565162951535312, 1.000000000000000000, 0.9510565162951535312, 1.000000000000000000, 0.9510565162951535312, 1.000000000000000000, 0.9510565162951535312, 1.000000000000000000, 0.9510565162951535312, 1.000000000000000000, 0.9510565162951535312, 1.000000000000000000, 0.9510565162951535312, 1.000000000000000000, 0.9510565162951535312, 1.000000000000000000, 0.9510565162951535312, 1.000000000000000000, 0.9510565162951535312, 1.000000000000000000, 0.9510565162951535312, 1.000000000000000000, 0.9510565162951535312, 1.000000000000000000, 0.9510565162951535312, 1.000000000000000000, 0.9510565162951535312, 1.000000000000000000, 0.9510565162951535312, 1.000000000000000000, 0.9510565162951535312, 1.000000000000000000, 0.9510565162951535312, 1.000000000000000000, 0.9510565162951535312, 1.000000000000000000, 0.9510565162951535312, 1.000000000000000000, 0.9510565162951535312, 1.000000000000000000, 0.9510565162951535312, 1.000000000000000000, 0.9510565162951535312, 1.000000000000000000, 0.9510565162951535312, 1.000000000000000000, 0.9510565162951535312, 1.000000000000000000, 0.9510565162951535312, 1.000000000000000000, 0.9510565162951535312, 1.000000000000000000, 0.9510565162951535312, 1.000000000000000000, 0.9510565162951535312, 1.000000000000000000, 0.9510565162951535312, 1.000000000000000000, 0.9510565162951535312, 1.000000000000000000, 0.9510565162951535312, 1.000000000000000000, 0.9510565162951535312, 1.000000000000000000, 0.9510565162951535312, 1.000000000000000000, 0.9510565162951535312, 1.000000000000000000, 0.9510565162951535312, 1.000000000000000000, 0.9510565162951535312, 1.000000000000000000, 0.9510565162951535312, 1.000000000000000000, 0.9510565162951535312, 1.000000000000000000, 0.9510565162951535312, 1.000000000000000000, 0.9510565162951535312, 1.000000000000000000, 0.9510565162951535312, 1.000000000000000000, 0.9510565162951535312, 1.000000000000000000, 0.9510565162951535312, 1.000000000000000000, 0.9510565162951535312, 1.000000000000000000, 0.9510565162951535312, 1.000000000000000000, 0.9510565162951535312, 1.000000000000000000, 0.9510565162951535312, 1.000000000000000000, 0.9510565162951535312, 1.000000000000000000, 0.9510565162951535312, 1.000000000000000000, 0.9510565162951535312, 1.000000000000000000, 0.9510565162951535312, 1.000000000000000000, 0.9510565162951535312, 1.000000000000000000, 0.9510565162951535312, 1.000000000000000000, 0.9510565162951535312, 1.000000000000000000, 0.9510565162951535312, 1.000000000000000000, 0.9510565162951535312, 1.000000000000000000, 0.9510565162951535312, 1.000000000000000000, 0.9510565162951535312, 1.000000000000000000, 0.9510565162951535312, 1.000000000000000000, 0.9510565162951535312, 1.000000000000000000, 0.9510565162951535312, 1.000000000000000000, 0.9510565162951535312, 1.000000000000000000, 0.9510565162951535312, 1.000000000000000000, 0.9510565162951535312, 1.000000000000000000, 0.9510565162951535312, 1.000000000000000000, 0.9510565162951535312, 1.000000000000000000, 0.9510565162951535312, 1.000000000000000000, 0.9510565162951535312, 1.000000000000000000, 0.9510565162951535312, 1.000000000000000000, 0.9510565162951535312, 1.000000000000000000 ) ) 
 REPRESENTATION_ITEM ( '' )  );
#15314 = CYLINDRICAL_SURFACE ( 'NONE', #1198, 0.5999999999999998668 ) ;
#15315 = LINE ( 'NONE', #15217, #14100 ) ;
#15316 = ADVANCED_FACE ( 'NONE', ( #15856 ), #8293, .T. ) ;
#15317 = SURFACE_STYLE_USAGE ( .BOTH. , #9326 ) ;
#15318 = STYLED_ITEM ( 'NONE', ( #1701 ), #8234 ) ;
#15319 = ORIENTED_EDGE ( 'NONE', *, *, #3792, .F. ) ;
#15320 = CARTESIAN_POINT ( 'NONE',  ( 6.466260427357672924, 2.904280683598007951, -5.030361703432632225 ) ) ;
#15321 = CARTESIAN_POINT ( 'NONE',  ( 45.86712807150329496, 47.70051614449766220, 5.649768623646139964 ) ) ;
#15322 = CIRCLE ( 'NONE', #17213, 6.000000000000000888 ) ;
#15323 = AXIS2_PLACEMENT_3D ( 'NONE', #16320, #8856, #4160 ) ;
#15324 = CARTESIAN_POINT ( 'NONE',  ( 47.74827507625478518, 64.59948385550239891, 7.007379884777227730 ) ) ;
#15325 = LINE ( 'NONE', #3271, #13669 ) ;
#15326 = ORIENTED_EDGE ( 'NONE', *, *, #18277, .T. ) ;
#15327 = CARTESIAN_POINT ( 'NONE',  ( 4.086262629614032527, -4.082406995609991540, -0.07093633357110748494 ) ) ;
#15328 = CARTESIAN_POINT ( 'NONE',  ( 0.1085714285714285687, -3.798448662927795372, -0.8000000000000000444 ) ) ;
#15329 = CARTESIAN_POINT ( 'NONE',  ( 44.88205777487398507, 61.19948385550241454, -3.688883143319540814 ) ) ;
#15330 = DIRECTION ( 'NONE',  ( 0.000000000000000000, 0.000000000000000000, 1.000000000000000000 ) ) ;
#15331 = FILL_AREA_STYLE ('',( #18003 ) ) ;
#15332 = CIRCLE ( 'NONE', #11878, 20.00000000000000000 ) ;
#15333 = CARTESIAN_POINT ( 'NONE',  ( 42.38452918213190657, 57.90051614449765793, 2.450534656007115508 ) ) ;
#15334 = CARTESIAN_POINT ( 'NONE',  ( 53.54508667620424234, 56.70051614449766930, -4.840751629271188961 ) ) ;
#15335 = CARTESIAN_POINT ( 'NONE',  ( 75.00000000000001421, -39.99999999999998579, -20.00000000000000000 ) ) ;
#15336 = CARTESIAN_POINT ( 'NONE',  ( -1.000000000000000222, -4.808326913195983821, 0.000000000000000000 ) ) ;
#15337 = AXIS2_PLACEMENT_3D ( 'NONE', #5115, #14126, #8340 ) ;
#15338 = VERTEX_POINT ( 'NONE', #5161 ) ;
#15339 = ORIENTED_EDGE ( 'NONE', *, *, #15270, .F. ) ;
#15340 = DIRECTION ( 'NONE',  ( 0.000000000000000000, 0.000000000000000000, 1.000000000000000000 ) ) ;
#15341 = ORIENTED_EDGE ( 'NONE', *, *, #1707, .T. ) ;
#15342 = LINE ( 'NONE', #6508, #8433 ) ;
#15343 = AXIS2_PLACEMENT_3D ( 'NONE', #7405, #16532, #7210 ) ;
#15344 = ORIENTED_EDGE ( 'NONE', *, *, #12504, .T. ) ;
#15345 = DIRECTION ( 'NONE',  ( 0.000000000000000000, 0.000000000000000000, 1.000000000000000000 ) ) ;
#15346 = CARTESIAN_POINT ( 'NONE',  ( 45.86712807150323812, 49.29948385550240175, -5.649768623646098220 ) ) ;
#15347 = ORIENTED_EDGE ( 'NONE', *, *, #12145, .F. ) ;
#15348 = DIRECTION ( 'NONE',  ( 0.000000000000000000, -1.000000000000000000, 8.673617379884035472E-16 ) ) ;
#15349 = EDGE_LOOP ( 'NONE', ( #16058, #18422, #6211, #3191 ) ) ;
#15350 = CARTESIAN_POINT ( 'NONE',  ( 43.20883090819745576, 54.79948385550240175, 4.963592699179006473 ) ) ;
#15351 = AXIS2_PLACEMENT_3D ( 'NONE', #1645, #161, #13497 ) ;
#15352 = CARTESIAN_POINT ( 'NONE',  ( 0.000000000000000000, 0.000000000000000000, 0.000000000000000000 ) ) ;
#15353 = CARTESIAN_POINT ( 'NONE',  ( 55.11794222512601493, 46.19948385550240744, 3.688883143319541702 ) ) ;
#15354 = CARTESIAN_POINT ( 'NONE',  ( 4.142654963991859951, 2.035398498734348305, -3.525413613457315076 ) ) ;
#15355 = CARTESIAN_POINT ( 'NONE',  ( 1.000000000000000444, -15.10102051443364246, 15.00000000000000355 ) ) ;
#15356 = AXIS2_PLACEMENT_3D ( 'NONE', #14972, #10261, #9089 ) ;
#15357 = CIRCLE ( 'NONE', #18493, 20.00000000000000000 ) ;
#15358 = CARTESIAN_POINT ( 'NONE',  ( 55.94051828345053679, 63.20051614449765509, 4.345558710429044069 ) ) ;
#15359 = DIRECTION ( 'NONE',  ( -1.000000000000000000, -0.000000000000000000, -0.000000000000000000 ) ) ;
#15360 = AXIS2_PLACEMENT_3D ( 'NONE', #507, #12457, #18469 ) ;
#15361 = CARTESIAN_POINT ( 'NONE',  ( 43.34962307344081012, 52.89948385550240317, 2.184720259617164650 ) ) ;
#15362 = CARTESIAN_POINT ( 'NONE',  ( 0.1999999999999987899, 0.000000000000000000, 3.500000000000000000 ) ) ;
#15363 = ORIENTED_EDGE ( 'NONE', *, *, #2084, .T. ) ;
#15364 = DIRECTION ( 'NONE',  ( -0.000000000000000000, 0.000000000000000000, -1.000000000000000000 ) ) ;
#15365 = AXIS2_PLACEMENT_3D ( 'NONE', #5585, #7254, #11555 ) ;
#15366 = CARTESIAN_POINT ( 'NONE',  ( 45.90387839640214196, 50.69948385550240744, 5.676469297603166098 ) ) ;
#15367 = DIRECTION ( 'NONE',  ( 1.000000000000000000, 0.000000000000000000, 0.000000000000000000 ) ) ;
#15368 = AXIS2_PLACEMENT_3D ( 'NONE', #7712, #376, #7907 ) ;
#15369 = CIRCLE ( 'NONE', #6585, 0.2000000000000000944 ) ;
#15370 = EDGE_LOOP ( 'NONE', ( #4344, #15344, #7298, #16251 ) ) ;
#15371 = AXIS2_PLACEMENT_3D ( 'NONE', #9922, #18780, #11300 ) ;
#15372 = CARTESIAN_POINT ( 'NONE',  ( 7.336184427528458230, 0.000000000000000000, 0.000000000000000000 ) ) ;
#15373 = ORIENTED_EDGE ( 'NONE', *, *, #3546, .F. ) ;
#15374 = CARTESIAN_POINT ( 'NONE',  ( 54.13287192849671214, 62.70051614449766220, -5.649768623646139964 ) ) ;
#15375 = ORIENTED_EDGE ( 'NONE', *, *, #7598, .F. ) ;
#15376 = CARTESIAN_POINT ( 'NONE',  ( 0.000000000000000000, 0.000000000000000000, 0.000000000000000000 ) ) ;
#15377 = UNCERTAINTY_MEASURE_WITH_UNIT (LENGTH_MEASURE( 1.000000000000000082E-05 ), #4479, 'distance_accuracy_value', 'NONE');
#15378 = DIRECTION ( 'NONE',  ( -1.000000000000000000, -1.387778780781445182E-16, -0.000000000000000000 ) ) ;
#15379 = CARTESIAN_POINT ( 'NONE',  ( 46.49166364869456913, 56.30051614449766362, -4.867452303228181343 ) ) ;
#15380 = CARTESIAN_POINT ( 'NONE',  ( 0.05140428708382594608, 3.841181488860376358, -3.346878500200759277 ) ) ;
#15381 = ADVANCED_FACE ( 'NONE', ( #15660 ), #11232, .F. ) ;
#15382 = CARTESIAN_POINT ( 'NONE',  ( -19.89043790736545603, -22.09056926535314602, -9.000000000000000000 ) ) ;
#15383 = DIRECTION ( 'NONE',  ( 0.8090169943749464521, 0.5877852522924744694, 0.000000000000000000 ) ) ;
#15384 = AXIS2_PLACEMENT_3D ( 'NONE', #5854, #15248, #11823 ) ;
#15385 = CARTESIAN_POINT ( 'NONE',  ( 56.79116909180259398, 59.20051614449766220, 4.963592699178938972 ) ) ;
#15386 = EDGE_CURVE ( 'NONE', #4669, #4718, #587, .T. ) ;
#15387 = VECTOR ( 'NONE', #126, 1000.000000000000000 ) ;
#15388 = VERTEX_POINT ( 'NONE', #6827 ) ;
#15389 = VERTEX_POINT ( 'NONE', #18816 ) ;
#15390 = CARTESIAN_POINT ( 'NONE',  ( 0.1085714285714285687, -3.798448662927795372, -0.8000000000000000444 ) ) ;
#15392 = ORIENTED_EDGE ( 'NONE', *, *, #11347, .F. ) ;
#15391 = EDGE_CURVE ( 'NONE', #11939, #18807, #14174, .T. ) ;
#15393 = EDGE_CURVE ( 'NONE', #14693, #1555, #11003, .T. ) ;
#15394 = PRODUCT_CONTEXT ( 'NONE', #13257, 'mechanical' ) ;
#15395 = ORIENTED_EDGE ( 'NONE', *, *, #14434, .T. ) ;
#15396 = CARTESIAN_POINT ( 'NONE',  ( -4.000000000000000000, 2.309401076758498483, -3.433295621305379353 ) ) ;
#15397 = CARTESIAN_POINT ( 'NONE',  ( 19.76107906696387673, -16.91783288752826664, 9.000000000000000000 ) ) ;
#15398 = DIRECTION ( 'NONE',  ( -0.000000000000000000, -0.000000000000000000, 1.000000000000000000 ) ) ;
#15399 = CIRCLE ( 'NONE', #1376, 5.000000000000000888 ) ;
#15400 = CARTESIAN_POINT ( 'NONE',  ( 4.071447262713888016, 4.041451884327382338, 0.000000000000000000 ) ) ;
#15401 = DIRECTION ( 'NONE',  ( -0.7071067811865533459, 0.000000000000000000, 0.7071067811865416886 ) ) ;
#15402 = EDGE_CURVE ( 'NONE', #16449, #1031, #7121, .T. ) ;
#15403 = DIRECTION ( 'NONE',  ( 0.1836763462126260738, -0.9829867750086873635, -1.521953536530129477E-22 ) ) ;
#15404 = EDGE_CURVE ( 'NONE', #2682, #10823, #2484, .T. ) ;
#15405 = CARTESIAN_POINT ( 'NONE',  ( 47.70284917648453415, 63.39948385550240317, -6.992620115222774047 ) ) ;
#15406 = FACE_OUTER_BOUND ( 'NONE', #19217, .T. ) ;
#15407 = CARTESIAN_POINT ( 'NONE',  ( 45.27934281921075410, 59.29948385550240886, -6.458785618021043895 ) ) ;
#15408 = CARTESIAN_POINT ( 'NONE',  ( 43.33558569842706021, 59.90051614449766504, 2.141517661632167169 ) ) ;
#15409 = FACE_BOUND ( 'NONE', #12202, .T. ) ;
#15410 = DIRECTION ( 'NONE',  ( 0.000000000000000000, 1.000000000000000000, 0.000000000000000000 ) ) ;
#15411 =( REPRESENTATION_RELATIONSHIP ('NONE','NONE', #16703, #11935 ) REPRESENTATION_RELATIONSHIP_WITH_TRANSFORMATION ( #6558 )SHAPE_REPRESENTATION_RELATIONSHIP( ) );
#15412 = ORIENTED_EDGE ( 'NONE', *, *, #15149, .T. ) ;
#15413 = CARTESIAN_POINT ( 'NONE',  ( 0.02944718078674397194, -0.6813962075909725247, -3.500000000000000000 ) ) ;
#15414 = CARTESIAN_POINT ( 'NONE',  ( 44.03140696652198471, 47.80051614449764941, 4.306917132069485454 ) ) ;
#15415 = CARTESIAN_POINT ( 'NONE',  ( 43.34962307344081012, 64.89948385550239607, 2.184720259617164650 ) ) ;
#15416 = AXIS2_PLACEMENT_3D ( 'NONE', #15645, #741, #839 ) ;
#15417 = CARTESIAN_POINT ( 'NONE',  ( 20.00000000000000000, -20.00000000000000000, -23.00000000000000000 ) ) ;
#15418 = ORIENTED_EDGE ( 'NONE', *, *, #10114, .T. ) ;
#15419 = CARTESIAN_POINT ( 'NONE',  ( 0.000000000000000000, 0.000000000000000000, 0.000000000000000000 ) ) ;
#15420 = DIRECTION ( 'NONE',  ( -0.000000000000000000, -0.000000000000000000, -1.000000000000000000 ) ) ;
#15421 = CARTESIAN_POINT ( 'NONE',  ( 48.07319477248768180, 60.59948385550240602, 6.007379884777225953 ) ) ;
#15422 = CARTESIAN_POINT ( 'NONE',  ( 14.17539641854931176, -34.10879641843979471, -9.000000000000000000 ) ) ;
#15423 = SURFACE_SIDE_STYLE ('',( #12673 ) ) ;
#15424 = ADVANCED_FACE ( 'NONE', ( #2439 ), #3803, .F. ) ;
#15425 =( BOUNDED_SURFACE ( )  B_SPLINE_SURFACE ( 3, 2, ( 
 ( #11400, #8266, #9929 ),
 ( #5232, #17214, #3965 ),
 ( #15732, #6800, #11310 ),
 ( #15830, #631, #18789 ),
 ( #5337, #5520, #8365 ),
 ( #8073, #17312, #4066 ) ),
 .UNSPECIFIED., .F., .F., .F. ) 
 B_SPLINE_SURFACE_WITH_KNOTS ( ( 4, 2, 4 ),
 ( 3, 3 ),
 ( 0.01651732063679904258, 0.01857756227444016389, 0.02063780391208128520 ),
 ( 0.000000000000000000, 1.000000000000000000 ),
 .UNSPECIFIED. ) 
 GEOMETRIC_REPRESENTATION_ITEM ( )  RATIONAL_B_SPLINE_SURFACE ( (
 ( 1.000000000000000000, 0.8047781231227483234, 1.000000000000000000),
 ( 1.000000000000000000, 0.8123782108664983070, 1.000000000000000000),
 ( 1.000000000000000000, 0.8190665102133478648, 1.000000000000000000),
 ( 1.000000000000000000, 0.8192358432844011329, 1.000000000000000000),
 ( 1.000000000000000000, 0.8126132624435309371, 1.000000000000000000),
 ( 1.000000000000000000, 0.8047712436238877443, 1.000000000000000000) ) ) 
 REPRESENTATION_ITEM ( '' )  SURFACE ( )  );
#15426 = DIRECTION ( 'NONE',  ( 0.000000000000000000, 0.000000000000000000, 1.000000000000000000 ) ) ;
#15427 = CARTESIAN_POINT ( 'NONE',  ( 43.20883090819742023, 58.20051614449766220, -4.963592699178938972 ) ) ;
#15428 = CARTESIAN_POINT ( 'NONE',  ( 52.29715082351538769, 44.60051614449766788, -6.992620115222796251 ) ) ;
#15429 = ADVANCED_FACE ( 'NONE', ( #14371 ), #955, .F. ) ;
#15430 = MANIFOLD_SOLID_BREP ( 'M5 Clearance Hole1', #18084 ) ;
#15431 = FACE_OUTER_BOUND ( 'NONE', #12935, .T. ) ;
#15432 = DIRECTION ( 'NONE',  ( 2.775466039758894710E-17, 2.253973589064049552E-19, -1.000000000000000000 ) ) ;
#15433 = VERTEX_POINT ( 'NONE', #4575 ) ;
#15434 = ORIENTED_EDGE ( 'NONE', *, *, #5327, .F. ) ;
#15435 = DIRECTION ( 'NONE',  ( 0.8090169943749546677, -0.5877852522924632561, 0.000000000000000000 ) ) ;
#15436 = VERTEX_POINT ( 'NONE', #14859 ) ;
#15437 = DIRECTION ( 'NONE',  ( 0.9829867750086872524, 0.1836763462126260182, -1.475957441759982183E-22 ) ) ;
#15438 = VERTEX_POINT ( 'NONE', #19410 ) ;
#15439 = DIRECTION ( 'NONE',  ( -1.000000000000000000, 0.000000000000000000, 0.000000000000000000 ) ) ;
#15440 = CARTESIAN_POINT ( 'NONE',  ( 47.70284917648453415, 53.39948385550239607, -6.992620115222774047 ) ) ;
#15441 = ADVANCED_FACE ( 'NONE', ( #11623 ), #17432, .T. ) ;
#15442 = VERTEX_POINT ( 'NONE', #16152 ) ;
#15443 = CARTESIAN_POINT ( 'NONE',  ( -1.150000000000000577, 0.000000000000000000, -5.899999999999999467 ) ) ;
#15444 = EDGE_LOOP ( 'NONE', ( #16437, #1039, #18738, #15395 ) ) ;
#15445 = CARTESIAN_POINT ( 'NONE',  ( 52.57664461997811856, 51.59948385550240602, -8.007379884777229506 ) ) ;
#15446 = FACE_OUTER_BOUND ( 'NONE', #6527, .T. ) ;
#15447 = EDGE_CURVE ( 'NONE', #1055, #6799, #18014, .T. ) ;
#15448 = CARTESIAN_POINT ( 'NONE',  ( 56.65037692655918988, 61.89948385550241028, -2.184720259617163762 ) ) ;
#15449 = CARTESIAN_POINT ( 'NONE',  ( 4.086376042167606748, 4.082715877136863902, -0.07147133206917800907 ) ) ;
#15450 = CARTESIAN_POINT ( 'NONE',  ( 0.000000000000000000, 0.000000000000000000, 0.000000000000000000 ) ) ;
#15451 = CARTESIAN_POINT ( 'NONE',  ( 47.74827507625469281, 62.40051614449766504, -7.007379884777203749 ) ) ;
#15452 = CARTESIAN_POINT ( 'NONE',  ( -62.49999999999997158, 32.50000000000001421, -9.999999999999998224 ) ) ;
#15453 = CARTESIAN_POINT ( 'NONE',  ( 57.36023556966787851, 59.99948385550240459, -0.02388180880522424582 ) ) ;
#15454 = CARTESIAN_POINT ( 'NONE',  ( -62.49999999999997158, 45.00000000000001421, -9.999999999999998224 ) ) ;
#15455 = ORIENTED_EDGE ( 'NONE', *, *, #19396, .T. ) ;
#15456 = EDGE_LOOP ( 'NONE', ( #10897, #11736, #13869, #19235, #13382, #7887 ) ) ;
#15457 = DIRECTION ( 'NONE',  ( 0.000000000000000000, 0.000000000000000000, 1.000000000000000000 ) ) ;
#15458 = AXIS2_PLACEMENT_3D ( 'NONE', #10617, #19292, #13372 ) ;
#15459 = CARTESIAN_POINT ( 'NONE',  ( 45.86712807150323812, 53.29948385550240886, -5.649768623646098220 ) ) ;
#15460 = CARTESIAN_POINT ( 'NONE',  ( -0.9999999999999995559, -15.10102051443364246, 15.00000000000000355 ) ) ;
#15461 = ORIENTED_EDGE ( 'NONE', *, *, #6290, .F. ) ;
#15462 = VECTOR ( 'NONE', #1019, 1000.000000000000000 ) ;
#15463 = FACE_OUTER_BOUND ( 'NONE', #17345, .T. ) ;
#15464 = ORIENTED_EDGE ( 'NONE', *, *, #12263, .T. ) ;
#15465 = DIRECTION ( 'NONE',  ( 0.000000000000000000, 0.000000000000000000, -1.000000000000000000 ) ) ;
#15466 = ORIENTED_EDGE ( 'NONE', *, *, #3522, .T. ) ;
#15467 = DIRECTION ( 'NONE',  ( -1.000000000000000000, 0.000000000000000000, -0.000000000000000000 ) ) ;
#15468 = DIRECTION ( 'NONE',  ( -0.000000000000000000, -0.000000000000000000, 1.000000000000000000 ) ) ;
#15469 = CARTESIAN_POINT ( 'NONE',  ( 55.08986747509849380, 63.20051614449766220, 3.727524721679155384 ) ) ;
#15470 = DIRECTION ( 'NONE',  ( 3.469446951953615175E-16, -1.000000000000000000, 0.000000000000000000 ) ) ;
#15471 = AXIS2_PLACEMENT_3D ( 'NONE', #7875, #2001, #18384 ) ;
#15472 = CARTESIAN_POINT ( 'NONE',  ( 0.000000000000000000, 0.4273491293402468805, 0.000000000000000000 ) ) ;
#15473 = CARTESIAN_POINT ( 'NONE',  ( 2.000000000000000000, 1.329782007511006281, 0.7677499999999984892 ) ) ;
#15474 = AXIS2_PLACEMENT_3D ( 'NONE', #6468, #6294, #12267 ) ;
#15475 = CARTESIAN_POINT ( 'NONE',  ( 43.20883090819742023, 58.20051614449766220, -4.963592699178938972 ) ) ;
#15476 = ORIENTED_EDGE ( 'NONE', *, *, #2477, .F. ) ;
#15477 = VERTEX_POINT ( 'NONE', #8973 ) ;
#15478 = CARTESIAN_POINT ( 'NONE',  ( 0.000000000000000000, 0.000000000000000000, 5.000000000000000000 ) ) ;
#15479 =( NAMED_UNIT ( * ) PLANE_ANGLE_UNIT ( ) SI_UNIT ( $, .RADIAN. ) );
#15480 = CARTESIAN_POINT ( 'NONE',  ( -19.99999999999999645, -20.00000000000000000, 9.000000000000000000 ) ) ;
#15481 = CONTEXT_DEPENDENT_SHAPE_REPRESENTATION ( #18069, #8519 ) ;
#15482 = ORIENTED_EDGE ( 'NONE', *, *, #15029, .T. ) ;
#15483 = DIRECTION ( 'NONE',  ( 0.000000000000000000, 0.000000000000000000, 1.000000000000000000 ) ) ;
#15484 = EDGE_CURVE ( 'NONE', #15338, #11405, #4037, .T. ) ;
#15485 = DIRECTION ( 'NONE',  ( 0.000000000000000000, 0.000000000000000000, -1.000000000000000000 ) ) ;
#15486 = VERTEX_POINT ( 'NONE', #19308 ) ;
#15487 = VECTOR ( 'NONE', #9964, 1000.000000000000000 ) ;
#15488 = ADVANCED_FACE ( 'NONE', ( #13493 ), #16442, .F. ) ;
#15489 = CARTESIAN_POINT ( 'NONE',  ( -11.75570504584937481, -36.18033988749900942, -9.000000000000000000 ) ) ;
#15490 = DIRECTION ( 'NONE',  ( 0.000000000000000000, 0.000000000000000000, 1.000000000000000000 ) ) ;
#15491 = DIRECTION ( 'NONE',  ( 1.000000000000000000, 0.000000000000000000, 0.000000000000000000 ) ) ;
#15492 = AXIS2_PLACEMENT_3D ( 'NONE', #3647, #18666, #6868 ) ;
#15493 = EDGE_CURVE ( 'NONE', #19111, #3032, #1858, .T. ) ;
#15494 = ADVANCED_FACE ( 'NONE', ( #11816 ), #4184, .F. ) ;
#15495 = DIRECTION ( 'NONE',  ( -0.000000000000000000, -0.000000000000000000, -1.000000000000000000 ) ) ;
#15496 = CARTESIAN_POINT ( 'NONE',  ( 44.03140696652192787, 63.19948385550240744, -4.306917132069425058 ) ) ;
#15497 = DIRECTION ( 'NONE',  ( 0.000000000000000000, 0.000000000000000000, 1.000000000000000000 ) ) ;
#15498 = CARTESIAN_POINT ( 'NONE',  ( 56.79116909180255135, 57.79948385550240175, -4.963592699179005585 ) ) ;
#15499 = CARTESIAN_POINT ( 'NONE',  ( 52.29715082351538769, 60.60051614449764656, -6.992620115222796251 ) ) ;
#15500 = EDGE_CURVE ( 'NONE', #7188, #11822, #7316, .T. ) ;
#15501 = AXIS2_PLACEMENT_3D ( 'NONE', #15074, #12024, #18025 ) ;
#15502 = CARTESIAN_POINT ( 'NONE',  ( -20.63749999999999929, 0.000000000000000000, 0.000000000000000000 ) ) ;
#15503 = FACE_OUTER_BOUND ( 'NONE', #2385, .T. ) ;
#15504 =( NAMED_UNIT ( * ) SI_UNIT ( $, .STERADIAN. ) SOLID_ANGLE_UNIT ( ) );
#15505 = ORIENTED_EDGE ( 'NONE', *, *, #14909, .F. ) ;
#15506 = DIRECTION ( 'NONE',  ( 0.000000000000000000, 0.000000000000000000, 1.000000000000000000 ) ) ;
#15507 = AXIS2_PLACEMENT_3D ( 'NONE', #10296, #2591, #16299 ) ;
#15508 = EDGE_CURVE ( 'NONE', #4677, #8297, #2731, .T. ) ;
#15509 = ADVANCED_FACE ( 'NONE', ( #13291 ), #10343, .F. ) ;
#15510 = DIRECTION ( 'NONE',  ( 1.000000000000000000, 0.000000000000000000, 0.000000000000000000 ) ) ;
#15511 = CARTESIAN_POINT ( 'NONE',  ( 54.89903213687075834, 44.74560054925188268, -5.000000000000007105 ) ) ;
#15512 = CARTESIAN_POINT ( 'NONE',  ( 4.158413352280813768, -2.044871626972823542, 3.541821552872969736 ) ) ;
#15513 = AXIS2_PLACEMENT_3D ( 'NONE', #6740, #2261, #12726 ) ;
#15514 = DIRECTION ( 'NONE',  ( 0.000000000000000000, 0.000000000000000000, 1.000000000000000000 ) ) ;
#15515 = ORIENTED_EDGE ( 'NONE', *, *, #9197, .T. ) ;
#15516 = LINE ( 'NONE', #9619, #8025 ) ;
#15517 = CARTESIAN_POINT ( 'NONE',  ( -0.9996874511566241628, -0.02500000000000071609, -9.000000000000000000 ) ) ;
#15518 = EDGE_CURVE ( 'NONE', #337, #11744, #15632, .T. ) ;
#15519 = CARTESIAN_POINT ( 'NONE',  ( 44.91013252490152752, 60.79948385550241596, 3.727524721679198461 ) ) ;
#15520 = CARTESIAN_POINT ( 'NONE',  ( 4.211140560182196957, -2.431303136016555122, -3.745885042887436622 ) ) ;
#15521 = CARTESIAN_POINT ( 'NONE',  ( 52.25172492374522903, 45.59948385550240602, -7.007379884777225953 ) ) ;
#15522 = DIRECTION ( 'NONE',  ( -1.000000000000000000, -0.000000000000000000, -0.000000000000000000 ) ) ;
#15523 = CARTESIAN_POINT ( 'NONE',  ( 41.58830220609386430, 60.00051614449765935, -0.02388180880514929535 ) ) ;
#15524 = AXIS2_PLACEMENT_3D ( 'NONE', #18243, #4797, #10760 ) ;
#15525 = CARTESIAN_POINT ( 'NONE',  ( 53.50833635130544508, 63.30051614449767072, 4.867452303228181343 ) ) ;
#15526 = DIRECTION ( 'NONE',  ( 1.000000000000000000, -0.000000000000000000, -0.000000000000000000 ) ) ;
#15527 = DIRECTION ( 'NONE',  ( -1.000000000000000000, 0.000000000000000000, 0.000000000000000000 ) ) ;
#15528 = ORIENTED_EDGE ( 'NONE', *, *, #1731, .F. ) ;
#15529=STYLED_ITEM('',(#19447),#1938);
#15530 = ORIENTED_EDGE ( 'NONE', *, *, #12998, .F. ) ;
#15531 = DIRECTION ( 'NONE',  ( 1.000000000000000000, 0.000000000000000000, 0.000000000000000000 ) ) ;
#15532 = EDGE_LOOP ( 'NONE', ( #14987, #13176, #2146, #12999 ) ) ;
#15533 = CARTESIAN_POINT ( 'NONE',  ( 4.050536630291690088, -2.401306687817039265, 2.976670123173768445 ) ) ;
#15534 = B_SPLINE_CURVE_WITH_KNOTS ( 'NONE', 3,
 ( #4221, #8630, #13239, #10099, #1192, #14703, #2959, #4322, #13329, #19250, #17762, #1093, #7358, #17476, #19349, #10290 ),
 .UNSPECIFIED., .F., .F.,
 ( 4, 3, 3, 3, 3, 4 ),
 ( -2.111273352581287704E-06, 0.000000000000000000, 3.519286887794526448E-05, 7.191842652068348909E-05, 0.0001049868727093649664, 0.0001382836236822123786 ),
 .UNSPECIFIED. ) ;
#15535 = ORIENTED_EDGE ( 'NONE', *, *, #406, .T. ) ;
#15536 = CARTESIAN_POINT ( 'NONE',  ( 2.000000000000000000, -1.502314598737159426E-15, -1.535500000000000087 ) ) ;
#15537 = CARTESIAN_POINT ( 'NONE',  ( 42.63976443033212149, 50.99948385550240459, 0.02388180880522514787 ) ) ;
#15538 = ORIENTED_EDGE ( 'NONE', *, *, #6433, .T. ) ;
#15539 = CARTESIAN_POINT ( 'NONE',  ( 6.495567275915079541, -2.917443832164891226, -5.053160945538031967 ) ) ;
#15540 = ORIENTED_EDGE ( 'NONE', *, *, #10935, .T. ) ;
#15541 = CARTESIAN_POINT ( 'NONE',  ( 43.18075615816989199, 51.19948385550240744, -4.924951120819313743 ) ) ;
#15542 = DIRECTION ( 'NONE',  ( 1.000000000000000000, -0.000000000000000000, 0.000000000000000000 ) ) ;
#15543 = CARTESIAN_POINT ( 'NONE',  ( 57.36023556966787851, 61.99948385550241170, -0.02388180880522424582 ) ) ;
#15544 = PLANE ( 'NONE',  #3842 ) ;
#15545 = CARTESIAN_POINT ( 'NONE',  ( 4.165266963751724560, -4.099263933823990236, 4.401844587977598791E-16 ) ) ;
#15546 = CARTESIAN_POINT ( 'NONE',  ( 54.13287192849671214, 58.70051614449765509, -5.649768623646139964 ) ) ;
#15547 = CARTESIAN_POINT ( 'NONE',  ( 45.86712807150323812, 57.29948385550240175, -5.649768623646098220 ) ) ;
#15548 = DIRECTION ( 'NONE',  ( -0.000000000000000000, -0.000000000000000000, 1.000000000000000000 ) ) ;
#15549 = AXIS2_PLACEMENT_3D ( 'NONE', #8251, #7874, #17099 ) ;
#15550 = DIRECTION ( 'NONE',  ( 1.000000000000000000, 0.000000000000000000, 0.000000000000000000 ) ) ;
#15551 = ORIENTED_EDGE ( 'NONE', *, *, #17858, .T. ) ;
#15552 = EDGE_CURVE ( 'NONE', #1096, #17210, #8687, .T. ) ;
#15553 = VERTEX_POINT ( 'NONE', #15061 ) ;
#15554 = CARTESIAN_POINT ( 'NONE',  ( 0.000000000000000000, 3.031088913245533867, 1.750000000000002887 ) ) ;
#15555 = SURFACE_STYLE_USAGE ( .BOTH. , #3698 ) ;
#15556 = EDGE_CURVE ( 'NONE', #4857, #17995, #1551, .T. ) ;
#15557 = TOROIDAL_SURFACE ( 'NONE', #19027, 4.100000000000000533, 0.1000000000000001582 ) ;
#15558 = CARTESIAN_POINT ( 'NONE',  ( 43.33558569842703179, 53.09948385550240602, -2.141517661632099223 ) ) ;
#15559 = B_SPLINE_CURVE_WITH_KNOTS ( 'NONE', 3,
 ( #12492, #18603, #18504, #8080, #17029, #7797, #3585, #15539, #14056, #638, #6615, #8180, #9644, #12692, #11213, #17219 ),
 .UNSPECIFIED., .F., .F.,
 ( 4, 3, 3, 3, 3, 4 ),
 ( -2.669610558406318528E-06, 0.000000000000000000, 5.703179328867203279E-05, 0.0001157653700806028548, 0.0001686517580799736817, 0.0002219032271235106112 ),
 .UNSPECIFIED. ) ;
#15560 = FILL_AREA_STYLE_COLOUR ( '', #2164 ) ;
#15561 = ORIENTED_EDGE ( 'NONE', *, *, #9285, .T. ) ;
#15562 = ORIENTED_EDGE ( 'NONE', *, *, #9148, .F. ) ;
#15563 = PLANE ( 'NONE',  #13020 ) ;
#15564 = AXIS2_PLACEMENT_3D ( 'NONE', #15835, #14541, #11696 ) ;
#15565 = ORIENTED_EDGE ( 'NONE', *, *, #3648, .T. ) ;
#15566 = CARTESIAN_POINT ( 'NONE',  ( -150.9999999999999716, -14.99999999999999645, 15.00000000000000000 ) ) ;
#15567 = ORIENTED_EDGE ( 'NONE', *, *, #525, .F. ) ;
#15568 = AXIS2_PLACEMENT_3D ( 'NONE', #12141, #18149, #13528 ) ;
#15569 = CARTESIAN_POINT ( 'NONE',  ( 50.02271294988512551, 46.49948385550240459, 7.000000000000000888 ) ) ;
#15570 = CARTESIAN_POINT ( 'NONE',  ( 4.000000000000000000, 0.3987449864460005378, -0.01220643443059817035 ) ) ;
#15571 = CARTESIAN_POINT ( 'NONE',  ( 46.49166364869456913, 60.30051614449767072, -4.867452303228181343 ) ) ;
#15572 = CARTESIAN_POINT ( 'NONE',  ( 0.000000000000000000, 4.330127018922190096, -2.500000000000006217 ) ) ;
#15573 = FILL_AREA_STYLE ('',( #8114 ) ) ;
#15574 = DIRECTION ( 'NONE',  ( -0.000000000000000000, -0.000000000000000000, 1.000000000000000000 ) ) ;
#15575 = VECTOR ( 'NONE', #4735, 1000.000000000000000 ) ;
#15576 = CARTESIAN_POINT ( 'NONE',  ( 57.61547081786810764, 58.90051614449766504, -2.450534656007114176 ) ) ;
#15577 = CIRCLE ( 'NONE', #560, 2.100000000000000089 ) ;
#15578 = ORIENTED_EDGE ( 'NONE', *, *, #4024, .T. ) ;
#15579 = ORIENTED_EDGE ( 'NONE', *, *, #10100, .F. ) ;
#15580 = DIRECTION ( 'NONE',  ( 0.000000000000000000, 0.000000000000000000, 1.000000000000000000 ) ) ;
#15581 = SURFACE_STYLE_FILL_AREA ( #6845 ) ;
#15582 = PRESENTATION_LAYER_ASSIGNMENT (  '', '', ( #10238 ) ) ;
#15583 = CARTESIAN_POINT ( 'NONE',  ( 2.449293598294706513E-15, -20.00000000000000000, 9.000000000000000000 ) ) ;
#15584 = ITEM_DEFINED_TRANSFORMATION ( 'NONE', 'NONE', #9986,  #10359 ) ;
#15585 = ORIENTED_EDGE ( 'NONE', *, *, #2455, .F. ) ;
#15586 = CYLINDRICAL_SURFACE ( 'NONE', #17091, 10.00000000000000888 ) ;
#15587 = CARTESIAN_POINT ( 'NONE',  ( 1.267864665261691752E-11, -20.00000000000000000, 9.999999999999998224 ) ) ;
#15588 = ORIENTED_EDGE ( 'NONE', *, *, #3820, .T. ) ;
#15589 = AXIS2_PLACEMENT_3D ( 'NONE', #17011, #617, #718 ) ;
#15590 = AXIS2_PLACEMENT_3D ( 'NONE', #2771, #16584, #16489 ) ;
#15591 = DIRECTION ( 'NONE',  ( 0.000000000000000000, 0.000000000000000000, -1.000000000000000000 ) ) ;
#15592 = CYLINDRICAL_SURFACE ( 'NONE', #4226, 1.999999999999998224 ) ;
#15593 = CARTESIAN_POINT ( 'NONE',  ( 14.00000000000000000, 15.00000000000001776, 9.000000000000000000 ) ) ;
#15594 = CARTESIAN_POINT ( 'NONE',  ( -4.211140560182196957, -2.431303136016552013, -3.745885042887436178 ) ) ;
#15595 = CARTESIAN_POINT ( 'NONE',  ( 53.50833635130540955, 45.69948385550240033, -4.867452303228209765 ) ) ;
#15596 = DIRECTION ( 'NONE',  ( 1.000000000000000000, 0.000000000000000000, 0.000000000000000000 ) ) ;
#15597 = CARTESIAN_POINT ( 'NONE',  ( 57.61547081786812896, 62.09948385550240602, 2.450534656007040901 ) ) ;
#15598 = ADVANCED_FACE ( 'NONE', ( #16538 ), #9067, .F. ) ;
#15599 = CARTESIAN_POINT ( 'NONE',  ( 54.13287192849671214, 62.70051614449766220, -5.649768623646139964 ) ) ;
#15600 = DIRECTION ( 'NONE',  ( 0.000000000000000000, 0.000000000000000000, 1.000000000000000000 ) ) ;
#15601 = VECTOR ( 'NONE', #5775, 1000.000000000000000 ) ;
#15602 = CIRCLE ( 'NONE', #10277, 1.000000000000000888 ) ;
#15603 = CARTESIAN_POINT ( 'NONE',  ( 0.000000000000000000, 0.000000000000000000, 0.000000000000000000 ) ) ;
#15604 = ORIENTED_EDGE ( 'NONE', *, *, #15081, .T. ) ;
#15605 = CARTESIAN_POINT ( 'NONE',  ( 2.000000000000000000, -0.8865213383406730374, -1.535499999999999421 ) ) ;
#15606 = DIRECTION ( 'NONE',  ( -0.000000000000000000, -0.000000000000000000, -1.000000000000000000 ) ) ;
#15607 = COLOUR_RGB ( '',1.000000000000000000, 0.9490196078431372140, 0.9098039215686274384 ) ;
#15608 = CARTESIAN_POINT ( 'NONE',  ( 45.86712807150329496, 51.70051614449766220, 5.649768623646139964 ) ) ;
#15609 = CARTESIAN_POINT ( 'NONE',  ( -20.00000000000000000, -19.99999999999999289, -12.00000000000000000 ) ) ;
#15610 = EDGE_CURVE ( 'NONE', #7574, #6925, #7791, .T. ) ;
#15611 = LINE ( 'NONE', #6312, #18705 ) ;
#15612 = VERTEX_POINT ( 'NONE', #1925 ) ;
#15613 = LINE ( 'NONE', #515, #14280 ) ;
#15614 = VECTOR ( 'NONE', #6254, 1000.000000000000000 ) ;
#15615 = DIRECTION ( 'NONE',  ( 0.000000000000000000, 0.000000000000000000, -1.000000000000000000 ) ) ;
#15616 = AXIS2_PLACEMENT_3D ( 'NONE', #14654, #2635, #11620 ) ;
#15617 = CARTESIAN_POINT ( 'NONE',  ( -0.9999999999999995559, -15.10102051443364246, -8.999999999999998224 ) ) ;
#15618 = CARTESIAN_POINT ( 'NONE',  ( 52.25172492374522903, 47.59948385550239891, -7.007379884777225953 ) ) ;
#15619 = DIRECTION ( 'NONE',  ( 1.000000000000000000, -0.000000000000000000, -0.000000000000000000 ) ) ;
#15620 = CARTESIAN_POINT ( 'NONE',  ( 42.38452918213190657, 59.90051614449767214, 2.450534656007115508 ) ) ;
#15621 = ADVANCED_FACE ( 'NONE', ( #13769 ), #7890, .F. ) ;
#15622 = CARTESIAN_POINT ( 'NONE',  ( 55.69932041026405045, 59.10051614449766078, 1.875703265242156359 ) ) ;
#15623 = EDGE_CURVE ( 'NONE', #8364, #18559, #8106, .T. ) ;
#15624 = STYLED_ITEM ( 'NONE', ( #1609 ), #18337 ) ;
#15625 = CARTESIAN_POINT ( 'NONE',  ( 14.86289650954800479, -33.38261212717704041, -9.000000000000000000 ) ) ;
#15626 = CARTESIAN_POINT ( 'NONE',  ( 6.507056549636238252, 2.993353539201078828, 4.999999999999999112 ) ) ;
#15627 = ORIENTED_EDGE ( 'NONE', *, *, #18878, .T. ) ;
#15628 = ORIENTED_EDGE ( 'NONE', *, *, #16666, .T. ) ;
#15629 = ORIENTED_EDGE ( 'NONE', *, *, #7288, .F. ) ;
#15630 = DIRECTION ( 'NONE',  ( -0.000000000000000000, -0.000000000000000000, -1.000000000000000000 ) ) ;
#15631 = VERTEX_POINT ( 'NONE', #12485 ) ;
#15632 = CIRCLE ( 'NONE', #9670, 20.00000000000000000 ) ;
#15633 = EDGE_CURVE ( 'NONE', #17671, #5344, #4770, .T. ) ;
#15634 = AXIS2_PLACEMENT_3D ( 'NONE', #6896, #6702, #5135 ) ;
#15635 = DIRECTION ( 'NONE',  ( -1.000000000000000000, 0.000000000000000000, 0.000000000000000000 ) ) ;
#15636 = ORIENTED_EDGE ( 'NONE', *, *, #9857, .T. ) ;
#15637 = DIRECTION ( 'NONE',  ( 0.000000000000000000, 0.000000000000000000, -1.000000000000000000 ) ) ;
#15638 = CARTESIAN_POINT ( 'NONE',  ( 50.02271294988512551, 60.49948385550240459, 7.000000000000000888 ) ) ;
#15639 = ORIENTED_EDGE ( 'NONE', *, *, #340, .T. ) ;
#15640 = DIRECTION ( 'NONE',  ( 0.02857142857142857054, 0.9995917534020515305, 0.000000000000000000 ) ) ;
#15641 = ORIENTED_EDGE ( 'NONE', *, *, #11076, .F. ) ;
#15642 = CARTESIAN_POINT ( 'NONE',  ( 58.41169779390614281, 53.99948385550241170, -0.02388180880523160798 ) ) ;
#15643 = CARTESIAN_POINT ( 'NONE',  ( -7.134732861516020819, -1.729090847147989773, -9.000000000000000000 ) ) ;
#15644 = CARTESIAN_POINT ( 'NONE',  ( 54.09612160359786515, 61.69948385550240744, -5.676469297603166098 ) ) ;
#15645 = CARTESIAN_POINT ( 'NONE',  ( -1.000000000000000000, -14.00000000000000000, 8.999999999999998224 ) ) ;
#15646 = DIRECTION ( 'NONE',  ( 0.03933706530295846826, -0.9992259981072103558, 7.446367396525005116E-17 ) ) ;
#15647 = CARTESIAN_POINT ( 'NONE',  ( 44.05948171654945611, 58.20051614449764799, -4.345558710429044069 ) ) ;
#15648 = VECTOR ( 'NONE', #1393, 1000.000000000000114 ) ;
#15649 = ADVANCED_FACE ( 'NONE', ( #9541 ), #15005, .T. ) ;
#15650 = CARTESIAN_POINT ( 'NONE',  ( 44.28664221472220675, 63.09948385550240602, -1.832500667257165317 ) ) ;
#15651 = EDGE_CURVE ( 'NONE', #18826, #13076, #18215, .T. ) ;
#15652 = CARTESIAN_POINT ( 'NONE',  ( 54.13287192849676188, 58.29948385550240175, 5.649768623646098220 ) ) ;
#15653 = CARTESIAN_POINT ( 'NONE',  ( -1.240299975428113101E-15, -4.647091401871173311, -3.572172305156514849 ) ) ;
#15654 = CARTESIAN_POINT ( 'NONE',  ( 6.323279575526007612, -3.325091652217148308, 4.240772318536393470 ) ) ;
#15655 = ORIENTED_EDGE ( 'NONE', *, *, #7350, .T. ) ;
#15656 = VECTOR ( 'NONE', #11329, 1000.000000000000000 ) ;
#15657 = ORIENTED_EDGE ( 'NONE', *, *, #14214, .F. ) ;
#15658 = FACE_OUTER_BOUND ( 'NONE', #5918, .T. ) ;
#15659 = CARTESIAN_POINT ( 'NONE',  ( 47.74827507625478518, 54.59948385550239180, 7.007379884777227730 ) ) ;
#15660 = FACE_OUTER_BOUND ( 'NONE', #2434, .T. ) ;
#15661 = VERTEX_POINT ( 'NONE', #15151 ) ;
#15662 = EDGE_LOOP ( 'NONE', ( #6509, #17184, #17693 ) ) ;
#15663 = CARTESIAN_POINT ( 'NONE',  ( -14.86289650954781649, -33.38261212717723936, 9.000000000000000000 ) ) ;
#15664 = AXIS2_PLACEMENT_3D ( 'NONE', #8788, #17727, #5754 ) ;
#15665 = ORIENTED_EDGE ( 'NONE', *, *, #9308, .T. ) ;
#15666 = VECTOR ( 'NONE', #12727, 1000.000000000000000 ) ;
#15667 = CARTESIAN_POINT ( 'NONE',  ( 1.250000000000001110, 0.000000000000000000, 0.000000000000000000 ) ) ;
#15668 = VECTOR ( 'NONE', #19113, 1000.000000000000227 ) ;
#15669 = ORIENTED_EDGE ( 'NONE', *, *, #4897, .T. ) ;
#15670 = EDGE_CURVE ( 'NONE', #15934, #18690, #2178, .T. ) ;
#15671 = CARTESIAN_POINT ( 'NONE',  ( 42.63976443033212860, 46.99948385550240459, 0.02388180880522514787 ) ) ;
#15672 = DIRECTION ( 'NONE',  ( -1.000000000000000000, -0.000000000000000000, -0.000000000000000000 ) ) ;
#15673 = CARTESIAN_POINT ( 'NONE',  ( 44.91013252490150620, 64.20051614449766930, -3.727524721679154940 ) ) ;
#15674 = CARTESIAN_POINT ( 'NONE',  ( -54.99999999999996447, -6.999999999999985789, -10.00000000000000000 ) ) ;
#15675 = EDGE_CURVE ( 'NONE', #19038, #18672, #8667, .T. ) ;
#15676 = DIRECTION ( 'NONE',  ( 0.000000000000000000, 0.000000000000000000, -1.000000000000000000 ) ) ;
#15677 = DIRECTION ( 'NONE',  ( 2.191393683118473446E-17, 7.538405132783725260E-17, 1.000000000000000000 ) ) ;
#15678 =( REPRESENTATION_RELATIONSHIP ('NONE','NONE', #16703, #8665 ) REPRESENTATION_RELATIONSHIP_WITH_TRANSFORMATION ( #8223 )SHAPE_REPRESENTATION_RELATIONSHIP( ) );
#15679 = AXIS2_PLACEMENT_3D ( 'NONE', #13711, #9108, #18048 ) ;
#15680 = AXIS2_PLACEMENT_3D ( 'NONE', #3596, #15548, #4786 ) ;
#15681 = CIRCLE ( 'NONE', #17577, 0.9999999999999995559 ) ;
#15682 = ORIENTED_EDGE ( 'NONE', *, *, #102, .T. ) ;
#15683 = ORIENTED_EDGE ( 'NONE', *, *, #19251, .T. ) ;
#15684 = FACE_OUTER_BOUND ( 'NONE', #9477, .T. ) ;
#15685 = CARTESIAN_POINT ( 'NONE',  ( 4.000000000000000000, -2.309401076758514915, -3.433295621305383349 ) ) ;
#15686 = ITEM_DEFINED_TRANSFORMATION ( 'NONE', 'NONE', #18779,  #10359 ) ;
#15687 = VECTOR ( 'NONE', #9424, 1000.000000000000000 ) ;
#15688 = ORIENTED_EDGE ( 'NONE', *, *, #2466, .T. ) ;
#15689 = CARTESIAN_POINT ( 'NONE',  ( -3.999999999999999112, 1.539600717838996324, -3.300726591567078039 ) ) ;
#15690 = PLANE ( 'NONE',  #10330 ) ;
#15691 = ORIENTED_EDGE ( 'NONE', *, *, #18929, .T. ) ;
#15692 = CIRCLE ( 'NONE', #13182, 20.00000000000000000 ) ;
#15693 = EDGE_CURVE ( 'NONE', #17210, #2254, #1822, .T. ) ;
#15694 = DIRECTION ( 'NONE',  ( 0.000000000000000000, 0.000000000000000000, -1.000000000000000000 ) ) ;
#15695 = CARTESIAN_POINT ( 'NONE',  ( 0.1404048886732821022, 4.699864953788070565, -3.686887068327037387 ) ) ;
#15696 = DIRECTION ( 'NONE',  ( 0.000000000000000000, 0.000000000000000000, -1.000000000000000000 ) ) ;
#15697 = VECTOR ( 'NONE', #16253, 1000.000000000000000 ) ;
#15698 = CIRCLE ( 'NONE', #18850, 4.000000000000031086 ) ;
#15699 = CARTESIAN_POINT ( 'NONE',  ( -6.259644161404860030E-16, -4.618802153517027165, -3.433295621305388234 ) ) ;
#15700 = CARTESIAN_POINT ( 'NONE',  ( 0.000000000000000000, 0.000000000000000000, 0.000000000000000000 ) ) ;
#15701 = CARTESIAN_POINT ( 'NONE',  ( 43.69122665457040000, 46.99948385550239749, 0.02388180880521036456 ) ) ;
#15702 = CARTESIAN_POINT ( 'NONE',  ( 3.799999999999999378, 0.000000000000000000, 0.000000000000000000 ) ) ;
#15703 = CARTESIAN_POINT ( 'NONE',  ( 54.13287192849676188, 48.29948385550240175, 5.649768623646098220 ) ) ;
#15704 = CARTESIAN_POINT ( 'NONE',  ( 55.96859303347802239, 62.80051614449766362, -4.306917132069484566 ) ) ;
#15705 = CARTESIAN_POINT ( 'NONE',  ( 20.00000000000000000, -20.00000000000000000, -23.00000000000000000 ) ) ;
#15706 = CYLINDRICAL_SURFACE ( 'NONE', #353, 4.000000000000031086 ) ;
#15707 = CARTESIAN_POINT ( 'NONE',  ( 0.000000000000000000, 0.000000000000000000, 0.000000000000000000 ) ) ;
#15708 = VERTEX_POINT ( 'NONE', #15243 ) ;
#15709 = CIRCLE ( 'NONE', #7256, 0.7500000000000000000 ) ;
#15710 = DIRECTION ( 'NONE',  ( -0.000000000000000000, -0.000000000000000000, 1.000000000000000000 ) ) ;
#15711 = VECTOR ( 'NONE', #19178, 1000.000000000000000 ) ;
#15712 = DIRECTION ( 'NONE',  ( 0.000000000000000000, 0.000000000000000000, 1.000000000000000000 ) ) ;
#15713 = CARTESIAN_POINT ( 'NONE',  ( 56.66441430157294690, 54.90051614449765793, -2.141517661632166281 ) ) ;
#15714 = CARTESIAN_POINT ( 'NONE',  ( 55.31939397794342028, 44.99999999999998579, -5.196074157289758411 ) ) ;
#15715 = PLANE ( 'NONE',  #11807 ) ;
#15716 = EDGE_LOOP ( 'NONE', ( #15636, #18135, #12759, #362, #7503 ) ) ;
#15717 = DIRECTION ( 'NONE',  ( -1.000000000000000000, 0.000000000000000000, 0.000000000000000000 ) ) ;
#15718 = LINE ( 'NONE', #5121, #2339 ) ;
#15719 = LINE ( 'NONE', #6400, #16226 ) ;
#15720 = CARTESIAN_POINT ( 'NONE',  ( 49.97728705011488159, 47.49948385550240459, -7.000000000000000888 ) ) ;
#15721 = CARTESIAN_POINT ( 'NONE',  ( 3.129923130707922496, -23.63917314727666152, -8.999999999999996447 ) ) ;
#15722 = CARTESIAN_POINT ( 'NONE',  ( 58.41169779390614281, 59.00051614449766646, 0.02388180880515032231 ) ) ;
#15723 = CARTESIAN_POINT ( 'NONE',  ( 49.97728705011494554, 63.50051614449765935, 6.000000000000000888 ) ) ;
#15724 = CARTESIAN_POINT ( 'NONE',  ( -74.99999999999997158, 32.50000000000001421, 15.00000000000000000 ) ) ;
#15725 = DIRECTION ( 'NONE',  ( -0.000000000000000000, -0.000000000000000000, -1.000000000000000000 ) ) ;
#15726 = ORIENTED_EDGE ( 'NONE', *, *, #14806, .F. ) ;
#15727 = ORIENTED_EDGE ( 'NONE', *, *, #18219, .F. ) ;
#15728 = VERTEX_POINT ( 'NONE', #10918 ) ;
#15729 = DIRECTION ( 'NONE',  ( 0.000000000000000000, 0.000000000000000000, 1.000000000000000000 ) ) ;
#15730 = EDGE_LOOP ( 'NONE', ( #17504, #12155, #581, #9859 ) ) ;
#15731 = B_SPLINE_CURVE_WITH_KNOTS ( 'NONE', 3,
 ( #15396, #15689, #18557, #2270, #8225 ),
 .UNSPECIFIED., .F., .F.,
 ( 4, 1, 4 ),
 ( 0.000000000000000000, 0.002309401076758505790, 0.004618802153517011580 ),
 .UNSPECIFIED. ) ;
#15732 = CARTESIAN_POINT ( 'NONE',  ( 3.880214671983734043, -0.7309020039772819999, 3.500000000000000444 ) ) ;
#15733 = VECTOR ( 'NONE', #9157, 1000.000000000000000 ) ;
#15734 = ORIENTED_EDGE ( 'NONE', *, *, #14235, .T. ) ;
#15735 = DIRECTION ( 'NONE',  ( 0.000000000000000000, 8.673617379884036458E-16, 1.000000000000000000 ) ) ;
#15736 = EDGE_CURVE ( 'NONE', #5817, #671, #16923, .T. ) ;
#15737 = CARTESIAN_POINT ( 'NONE',  ( 44.05948171654949874, 58.79948385550240175, 4.345558710429104465 ) ) ;
#15738 = ORIENTED_EDGE ( 'NONE', *, *, #3836, .F. ) ;
#15739 = DIRECTION ( 'NONE',  ( 0.000000000000000000, 0.000000000000000000, -1.000000000000000000 ) ) ;
#15740 = ORIENTED_EDGE ( 'NONE', *, *, #16491, .F. ) ;
#15741 = CARTESIAN_POINT ( 'NONE',  ( 47.37792948025162332, 51.39948385550241028, -7.992620115222770494 ) ) ;
#15742 = PRODUCT_RELATED_PRODUCT_CATEGORY ( 'part', '', ( #17923 ) ) ;
#15743 = DIRECTION ( 'NONE',  ( 0.000000000000000000, 0.000000000000000000, -1.000000000000000000 ) ) ;
#15744 = ADVANCED_FACE ( 'NONE', ( #12105 ), #4859, .T. ) ;
#15745 = CARTESIAN_POINT ( 'NONE',  ( 48.02776887271745210, 49.39948385550241028, -5.992620115222778487 ) ) ;
#15746 = DIRECTION ( 'NONE',  ( 1.000000000000000000, 0.000000000000000000, 0.000000000000000000 ) ) ;
#15747 = DIRECTION ( 'NONE',  ( 0.000000000000000000, -0.5000000000000011102, -0.8660254037844379305 ) ) ;
#15748 = CARTESIAN_POINT ( 'NONE',  ( 43.33558569842706021, 61.90051614449766504, 2.141517661632167169 ) ) ;
#15749 = EDGE_CURVE ( 'NONE', #2802, #9948, #2016, .T. ) ;
#15750 = CARTESIAN_POINT ( 'NONE',  ( 53.50833635130544508, 45.30051614449766362, 4.867452303228181343 ) ) ;
#15751 = EDGE_CURVE ( 'NONE', #2682, #9345, #15342, .T. ) ;
#15752 = CARTESIAN_POINT ( 'NONE',  ( 56.65037692655918988, 57.89948385550240317, -2.184720259617163762 ) ) ;
#15753 = FACE_OUTER_BOUND ( 'NONE', #9860, .T. ) ;
#15754 = CYLINDRICAL_SURFACE ( 'NONE', #19140, 0.9999999999999991118 ) ;
#15755 = ORIENTED_EDGE ( 'NONE', *, *, #11418, .T. ) ;
#15756 = EDGE_CURVE ( 'NONE', #2874, #6953, #13673, .T. ) ;
#15757 = PRODUCT_DEFINITION_FORMATION_WITH_SPECIFIED_SOURCE ( 'ANY', '', #14273, .NOT_KNOWN. ) ;
#15758 = ORIENTED_EDGE ( 'NONE', *, *, #7587, .T. ) ;
#15759 = LINE ( 'NONE', #11426, #16882 ) ;
#15760 = APPLICATION_PROTOCOL_DEFINITION ( 'draft international standard', 'automotive_design', 1998, #8769 ) ;
#15761 = ORIENTED_EDGE ( 'NONE', *, *, #13409, .F. ) ;
#15762 = CARTESIAN_POINT ( 'NONE',  ( 55.96859303347804371, 58.19948385550241454, 4.306917132069425946 ) ) ;
#15763 = CARTESIAN_POINT ( 'NONE',  ( 20.00000000000000000, -20.00000000000000000, -23.00000000000000000 ) ) ;
#15764 = VERTEX_POINT ( 'NONE', #6134 ) ;
#15765 = ORIENTED_EDGE ( 'NONE', *, *, #13610, .T. ) ;
#15766 = CARTESIAN_POINT ( 'NONE',  ( 20.00000000000000000, -14.99999999999999289, -20.00000000000000000 ) ) ;
#15767 = EDGE_CURVE ( 'NONE', #6603, #3135, #10301, .T. ) ;
#15768 = ADVANCED_FACE ( 'NONE', ( #9171 ), #15425, .F. ) ;
#15769 = ORIENTED_EDGE ( 'NONE', *, *, #4601, .F. ) ;
#15770 = CARTESIAN_POINT ( 'NONE',  ( 0.000000000000000000, 20.00000000000001421, 9.999999999999998224 ) ) ;
#15771 = VERTEX_POINT ( 'NONE', #6995 ) ;
#15772 = CARTESIAN_POINT ( 'NONE',  ( 54.13287192849676188, 48.29948385550240175, 5.649768623646098220 ) ) ;
#15773 = FACE_OUTER_BOUND ( 'NONE', #98, .T. ) ;
#15774 = CARTESIAN_POINT ( 'NONE',  ( 44.88205777487401349, 63.80051614449766362, 3.688883143319584779 ) ) ;
#15775 = CARTESIAN_POINT ( 'NONE',  ( -44.99999999999997158, -40.00000000000000000, -10.00000000000000000 ) ) ;
#15776 = FILL_AREA_STYLE_COLOUR ( '', #3948 ) ;
#15777 = PLANE ( 'NONE',  #4716 ) ;
#15778 = AXIS2_PLACEMENT_3D ( 'NONE', #11608, #18898, #1226 ) ;
#15779 = ORIENTED_EDGE ( 'NONE', *, *, #11164, .F. ) ;
#15780 = ORIENTED_EDGE ( 'NONE', *, *, #7284, .F. ) ;
#15781 = DIRECTION ( 'NONE',  ( 0.000000000000000000, 0.000000000000000000, 1.000000000000000000 ) ) ;
#15782 = CIRCLE ( 'NONE', #6086, 2.000000000000001776 ) ;
#15783 = DIRECTION ( 'NONE',  ( 1.000000000000000000, 0.000000000000000000, 0.000000000000000000 ) ) ;
#15784 = CARTESIAN_POINT ( 'NONE',  ( -154.8605857259444463, -18.79744172571344762, 15.79999999999999893 ) ) ;
#15785 = CONTEXT_DEPENDENT_SHAPE_REPRESENTATION ( #19076, #6777 ) ;
#15786 = VERTEX_POINT ( 'NONE', #6609 ) ;
#15787 = DIRECTION ( 'NONE',  ( 0.000000000000000000, 0.000000000000000000, 1.000000000000000000 ) ) ;
#15788 = ORIENTED_EDGE ( 'NONE', *, *, #16280, .F. ) ;
#15789 = AXIS2_PLACEMENT_3D ( 'NONE', #18480, #517, #16808 ) ;
#15790 = CARTESIAN_POINT ( 'NONE',  ( 5.599999999999998757, 0.000000000000000000, 0.000000000000000000 ) ) ;
#15791 = CARTESIAN_POINT ( 'NONE',  ( 6.355324643801638196, 1.972141403783284730, -5.108685331087993831 ) ) ;
#15792 = VECTOR ( 'NONE', #18563, 1000.000000000000000 ) ;
#15793 = CARTESIAN_POINT ( 'NONE',  ( -74.99999999999997158, 20.00000000000001421, 15.00000000000000000 ) ) ;
#15794 = CARTESIAN_POINT ( 'NONE',  ( 4.151274195509679465, 2.039912954708742898, 3.533232880573493606 ) ) ;
#15795 = CARTESIAN_POINT ( 'NONE',  ( 51.97223112728254790, 50.39948385550241738, 5.992620115222778487 ) ) ;
#15796 = CARTESIAN_POINT ( 'NONE',  ( 45.15499999999999403, 0.000000000000000000, 2.500000000000000444 ) ) ;
#15797 = CARTESIAN_POINT ( 'NONE',  ( 47.37792948025162332, 65.39948385550239607, -7.992620115222770494 ) ) ;
#15798 = CARTESIAN_POINT ( 'NONE',  ( 43.33558569842706021, 61.90051614449766504, 2.141517661632167169 ) ) ;
#15799 = CARTESIAN_POINT ( 'NONE',  ( 0.1999999999999987899, 4.041334437186265510E-16, -3.299999999999999822 ) ) ;
#15800 = CARTESIAN_POINT ( 'NONE',  ( 6.327632967270859332, 5.346704644972003706, -0.7392359018481428068 ) ) ;
#15801 = ADVANCED_FACE ( 'NONE', ( #3869 ), #12887, .T. ) ;
#15802 = DIRECTION ( 'NONE',  ( 1.000000000000000000, 0.000000000000000000, 0.000000000000000000 ) ) ;
#15803 = EDGE_LOOP ( 'NONE', ( #12684, #907, #8272, #7985 ) ) ;
#15804 = VECTOR ( 'NONE', #291, 1000.000000000000000 ) ;
#15805 = DIRECTION ( 'NONE',  ( 0.4999999999999974465, 0.8660254037844401509, 0.000000000000000000 ) ) ;
#15806 = EDGE_CURVE ( 'NONE', #17098, #3997, #925, .T. ) ;
#15807 = DIRECTION ( 'NONE',  ( 0.000000000000000000, 0.000000000000000000, -1.000000000000000000 ) ) ;
#15808 = CARTESIAN_POINT ( 'NONE',  ( 52.25172492374528588, 55.40051614449765083, 7.007379884777204637 ) ) ;
#15809 = VECTOR ( 'NONE', #1534, 1000.000000000000000 ) ;
#15810 = CARTESIAN_POINT ( 'NONE',  ( 4.175326769692855322, -2.060699556488924333, 3.569236330973470928 ) ) ;
#15811 = DIRECTION ( 'NONE',  ( 0.000000000000000000, 0.000000000000000000, -1.000000000000000000 ) ) ;
#15812 = ORIENTED_EDGE ( 'NONE', *, *, #19249, .T. ) ;
#15813 = CARTESIAN_POINT ( 'NONE',  ( 3.948103430090711630, -2.682758828852738642, 2.353325403972896357 ) ) ;
#15814 = CARTESIAN_POINT ( 'NONE',  ( 1.925929944387235853E-31, 15.00000000000001599, 15.00000000000000000 ) ) ;
#15815 = DIRECTION ( 'NONE',  ( 1.000000000000000000, 0.000000000000000000, 0.000000000000000000 ) ) ;
#15816 = FACE_OUTER_BOUND ( 'NONE', #830, .T. ) ;
#15817 = VECTOR ( 'NONE', #3930, 1000.000000000000000 ) ;
#15818 = DIRECTION ( 'NONE',  ( 0.000000000000000000, -1.000000000000000000, 0.000000000000000000 ) ) ;
#15819 = CARTESIAN_POINT ( 'NONE',  ( 47.37792948025170858, 63.60051614449764656, 7.992620115222797139 ) ) ;
#15820 = AXIS2_PLACEMENT_3D ( 'NONE', #6061, #1161, #5666 ) ;
#15821 = SURFACE_STYLE_USAGE ( .BOTH. , #11778 ) ;
#15822 = CARTESIAN_POINT ( 'NONE',  ( 55.69932041026405045, 63.10051614449766078, 1.875703265242156359 ) ) ;
#15823 = LINE ( 'NONE', #9534, #17895 ) ;
#15824 = PLANE ( 'NONE',  #16941 ) ;
#15825 = CIRCLE ( 'NONE', #7056, 2.000000000000001332 ) ;
#15826 = ORIENTED_EDGE ( 'NONE', *, *, #1640, .T. ) ;
#15827 = EDGE_LOOP ( 'NONE', ( #7916, #9406, #36, #7895 ) ) ;
#15828 = FACE_OUTER_BOUND ( 'NONE', #17286, .T. ) ;
#15829 = ORIENTED_EDGE ( 'NONE', *, *, #5984, .T. ) ;
#15830 = CARTESIAN_POINT ( 'NONE',  ( 3.878089031707363521, 0.7015470581914173831, 3.500000000000000444 ) ) ;
#15831 = VERTEX_POINT ( 'NONE', #2216 ) ;
#15832 = CARTESIAN_POINT ( 'NONE',  ( 2.000000000000000000, 0.8865213383406680414, -1.535500000000000975 ) ) ;
#15833 = CARTESIAN_POINT ( 'NONE',  ( 47.74827507625477807, 58.59948385550239180, 7.007379884777229506 ) ) ;
#15834 = EDGE_LOOP ( 'NONE', ( #8978, #18160, #10029, #18197 ) ) ;
#15835 = CARTESIAN_POINT ( 'NONE',  ( -62.49999999999997158, 32.50000000000001421, 15.00000000000000000 ) ) ;
#15836 = ORIENTED_EDGE ( 'NONE', *, *, #11057, .F. ) ;
#15837 = CARTESIAN_POINT ( 'NONE',  ( 42.39856655714566358, 56.89948385550240317, 2.493737253992119207 ) ) ;
#15838 = DIRECTION ( 'NONE',  ( -0.000000000000000000, 1.000000000000000000, -0.000000000000000000 ) ) ;
#15839 = CARTESIAN_POINT ( 'NONE',  ( 46.49166364869460466, 50.69948385550240744, 4.867452303228209765 ) ) ;
#15840 = CARTESIAN_POINT ( 'NONE',  ( 6.367873360227559232, -5.773502691896263528, 0.000000000000000000 ) ) ;
#15841 = CARTESIAN_POINT ( 'NONE',  ( 2.449293598294706513E-15, -20.00000000000000000, 9.000000000000000000 ) ) ;
#15842 = CARTESIAN_POINT ( 'NONE',  ( 42.63976443033212860, 64.00051614449765225, -0.02388180880514948964 ) ) ;
#15843 = CARTESIAN_POINT ( 'NONE',  ( 55.69932041026404335, 61.89948385550241738, -1.875703265242203432 ) ) ;
#15844 = CIRCLE ( 'NONE', #13026, 20.00000000000000000 ) ;
#15845 = CARTESIAN_POINT ( 'NONE',  ( 1.925929944387235853E-31, 15.00000000000001599, 9.000000000000000000 ) ) ;
#15846 = CARTESIAN_POINT ( 'NONE',  ( -154.9999999999999716, -14.99999999999999645, 15.79999999999999893 ) ) ;
#15847 = EDGE_CURVE ( 'NONE', #1920, #14655, #4048, .T. ) ;
#15848 = ORIENTED_EDGE ( 'NONE', *, *, #9867, .T. ) ;
#15849 = EDGE_LOOP ( 'NONE', ( #10153, #3604, #2965, #2704, #13557, #2158, #5540, #1951, #11994, #11316, #17792, #17717, #1071, #307, #16733, #3618 ) ) ;
#15850 = CARTESIAN_POINT ( 'NONE',  ( 0.000000000000000000, 0.000000000000000000, 0.000000000000000000 ) ) ;
#15851 =( LENGTH_UNIT ( ) NAMED_UNIT ( * ) SI_UNIT ( .MILLI., .METRE. ) );
#15852 = ORIENTED_EDGE ( 'NONE', *, *, #8813, .F. ) ;
#15853 = PRODUCT_RELATED_PRODUCT_CATEGORY ( 'part', '', ( #13052 ) ) ;
#15854 = VECTOR ( 'NONE', #15859, 1000.000000000000114 ) ;
#15855 = CARTESIAN_POINT ( 'NONE',  ( 56.65037692655918988, 59.89948385550241028, -2.184720259617163762 ) ) ;
#15856 = FACE_OUTER_BOUND ( 'NONE', #2869, .T. ) ;
#15857 = VERTEX_POINT ( 'NONE', #8174 ) ;
#15858 = ORIENTED_EDGE ( 'NONE', *, *, #15651, .F. ) ;
#15859 = DIRECTION ( 'NONE',  ( 0.000000000000000000, -0.5000000000000011102, -0.8660254037844379305 ) ) ;
#15860 = PRODUCT ( 'MAS-177', 'MAS-177', '', ( #17528 ) ) ;
#15861 = VERTEX_POINT ( 'NONE', #3775 ) ;
#15862 = FACE_OUTER_BOUND ( 'NONE', #17381, .T. ) ;
#15863 = ORIENTED_EDGE ( 'NONE', *, *, #17794, .F. ) ;
#15864 = CARTESIAN_POINT ( 'NONE',  ( 55.94051828345050836, 53.79948385550238754, -4.345558710429104465 ) ) ;
#15865 = DIRECTION ( 'NONE',  ( 0.000000000000000000, -0.000000000000000000, 1.000000000000000000 ) ) ;
#15866 = ADVANCED_FACE ( 'NONE', ( #14245 ), #12588, .F. ) ;
#15867 = AXIS2_PLACEMENT_3D ( 'NONE', #15041, #16623, #9237 ) ;
#15868 = CARTESIAN_POINT ( 'NONE',  ( 44.03140696652198471, 45.80051614449764230, 4.306917132069485454 ) ) ;
#15869 = DIRECTION ( 'NONE',  ( -0.000000000000000000, -0.000000000000000000, -1.000000000000000000 ) ) ;
#15870 = CARTESIAN_POINT ( 'NONE',  ( -3.158233816355059620, -39.56295201467614220, -9.000000000000000000 ) ) ;
#15871 = EDGE_CURVE ( 'NONE', #19334, #1202, #14035, .T. ) ;
#15872 = EDGE_CURVE ( 'NONE', #14264, #17671, #18889, .T. ) ;
#15873 = VERTEX_POINT ( 'NONE', #12973 ) ;
#15874 = ORIENTED_EDGE ( 'NONE', *, *, #11792, .T. ) ;
#15875 = LINE ( 'NONE', #2659, #2789 ) ;
#15876 = AXIS2_PLACEMENT_3D ( 'NONE', #1805, #15514, #612 ) ;
#15877 = LINE ( 'NONE', #8412, #19363 ) ;
#15878 = LINE ( 'NONE', #15784, #16244 ) ;
#15879 = ITEM_DEFINED_TRANSFORMATION ( 'NONE', 'NONE', #15012,  #10359 ) ;
#15880 = ORIENTED_EDGE ( 'NONE', *, *, #12987, .F. ) ;
#15881 = VECTOR ( 'NONE', #3853, 1000.000000000000000 ) ;
#15882 = CARTESIAN_POINT ( 'NONE',  ( 6.207671477328661425, 5.338259717474330479, 0.7538629453361838095 ) ) ;
#15883 = EDGE_CURVE ( 'NONE', #8263, #18115, #2623, .T. ) ;
#15885 = EDGE_CURVE ( 'NONE', #15661, #1247, #2812, .T. ) ;
#15884 = ORIENTED_EDGE ( 'NONE', *, *, #4788, .T. ) ;
#15886 = EDGE_CURVE ( 'NONE', #12908, #7823, #14147, .T. ) ;
#15887 = CARTESIAN_POINT ( 'NONE',  ( -129.9999999999999716, -14.99999999999999645, 9.000000000000000000 ) ) ;
#15888 = CARTESIAN_POINT ( 'NONE',  ( 4.175813232069148562, 4.122719923832741884, -2.765695189283172261E-17 ) ) ;
#15889 = CARTESIAN_POINT ( 'NONE',  ( 50.02271294988511841, 62.49948385550240459, 6.000000000000000888 ) ) ;
#15890 = CARTESIAN_POINT ( 'NONE',  ( -59.84999999999998721, 32.50000000000001421, -9.999999999999998224 ) ) ;
#15891 = CIRCLE ( 'NONE', #17469, 0.5999999999999998668 ) ;
#15892 = DIRECTION ( 'NONE',  ( 1.000000000000000000, 0.000000000000000000, 0.000000000000000000 ) ) ;
#15893 = CARTESIAN_POINT ( 'NONE',  ( 53.54508667620428497, 50.29948385550240886, 4.840751629271157874 ) ) ;
#15894 = CARTESIAN_POINT ( 'NONE',  ( 3.951447005078454477, -3.704664227300105583, -0.5833333333333333703 ) ) ;
#15895 = AXIS2_PLACEMENT_3D ( 'NONE', #18511, #942, #8086 ) ;
#15896 = CARTESIAN_POINT ( 'NONE',  ( 43.34962307344081012, 48.89948385550240317, 2.184720259617164650 ) ) ;
#15897 = CARTESIAN_POINT ( 'NONE',  ( 42.39856655714564226, 46.10051614449766078, -2.493737253992044156 ) ) ;
#15898 = FACE_OUTER_BOUND ( 'NONE', #17048, .T. ) ;
#15899 = CARTESIAN_POINT ( 'NONE',  ( 1.567478505476134606E-15, 4.618802153517012066, -3.433295621305382905 ) ) ;
#15900 = DIRECTION ( 'NONE',  ( -0.7779254092217071648, -0.6283566325640552730, 1.130512422757410501E-16 ) ) ;
#15901 = AXIS2_PLACEMENT_3D ( 'NONE', #13549, #11872, #122 ) ;
#15902 = ORIENTED_EDGE ( 'NONE', *, *, #13389, .F. ) ;
#15903 = FACE_OUTER_BOUND ( 'NONE', #826, .T. ) ;
#15904 = CIRCLE ( 'NONE', #8704, 4.000000000000031086 ) ;
#15905 = DIRECTION ( 'NONE',  ( -9.858538378746663627E-23, 5.031452844637890958E-23, -1.000000000000000000 ) ) ;
#15906 = CARTESIAN_POINT ( 'NONE',  ( 52.25172492374528588, 51.40051614449767214, 7.007379884777204637 ) ) ;
#15907 = DIRECTION ( 'NONE',  ( -1.000000000000000000, 0.000000000000000000, 0.000000000000000000 ) ) ;
#15908 = DIRECTION ( 'NONE',  ( 0.9999419836444144449, 0.01077169184824096695, 0.000000000000000000 ) ) ;
#15909 = VERTEX_POINT ( 'NONE', #12687 ) ;
#15910 = DIRECTION ( 'NONE',  ( 0.000000000000000000, -0.000000000000000000, 1.000000000000000000 ) ) ;
#15911 = DIRECTION ( 'NONE',  ( 0.000000000000000000, 0.000000000000000000, -1.000000000000000000 ) ) ;
#15912 = EDGE_CURVE ( 'NONE', #12436, #2611, #18688, .T. ) ;
#15913 = DIRECTION ( 'NONE',  ( 2.191393683118470056E-17, 7.538405132783724027E-17, 1.000000000000000000 ) ) ;
#15914 = CARTESIAN_POINT ( 'NONE',  ( 57.36023556966787851, 51.99948385550238328, -0.02388180880522424582 ) ) ;
#15915 = PLANE ( 'NONE',  #5759 ) ;
#15916 = CARTESIAN_POINT ( 'NONE',  ( 42.38452918213190657, 63.90051614449765793, 2.450534656007115508 ) ) ;
#15917 =( LENGTH_UNIT ( ) NAMED_UNIT ( * ) SI_UNIT ( .MILLI., .METRE. ) );
#15918 =( GEOMETRIC_REPRESENTATION_CONTEXT ( 3 ) GLOBAL_UNCERTAINTY_ASSIGNED_CONTEXT ( ( #17753 ) ) GLOBAL_UNIT_ASSIGNED_CONTEXT ( ( #3035, #1459, #16468 ) ) REPRESENTATION_CONTEXT ( 'NONE', 'WORKASPACE' ) );
#15919 = EDGE_CURVE ( 'NONE', #17135, #5826, #12822, .T. ) ;
#15920 = CARTESIAN_POINT ( 'NONE',  ( 54.09612160359792199, 51.30051614449766362, 5.676469297603124353 ) ) ;
#15921 = CIRCLE ( 'NONE', #6216, 5.000000000000000888 ) ;
#15922 = DIRECTION ( 'NONE',  ( -0.000000000000000000, 0.000000000000000000, 1.000000000000000000 ) ) ;
#15923 = DIRECTION ( 'NONE',  ( 1.000000000000000000, 0.000000000000000000, 0.000000000000000000 ) ) ;
#15924 = ORIENTED_EDGE ( 'NONE', *, *, #15518, .F. ) ;
#15925 = STYLED_ITEM ( 'NONE', ( #16979 ), #16200 ) ;
#15926 = ORIENTED_EDGE ( 'NONE', *, *, #3886, .T. ) ;
#15927 = DIRECTION ( 'NONE',  ( 1.000000000000000000, 0.000000000000000000, -0.000000000000000000 ) ) ;
#15928 = ORIENTED_EDGE ( 'NONE', *, *, #15556, .T. ) ;
#15929 = CARTESIAN_POINT ( 'NONE',  ( 6.355324643801635531, -1.972141403783270075, 5.108685331087992942 ) ) ;
#15930 = ORIENTED_EDGE ( 'NONE', *, *, #14651, .F. ) ;
#15931 = DIRECTION ( 'NONE',  ( 0.000000000000000000, 0.000000000000000000, 1.000000000000000000 ) ) ;
#15932 = CARTESIAN_POINT ( 'NONE',  ( 50.02271294988512551, 56.49948385550240459, 7.000000000000000888 ) ) ;
#15933 = AXIS2_PLACEMENT_3D ( 'NONE', #1947, #6530, #9562 ) ;
#15934 = VERTEX_POINT ( 'NONE', #13174 ) ;
#15935 = FACE_OUTER_BOUND ( 'NONE', #9052, .T. ) ;
#15936 = ORIENTED_EDGE ( 'NONE', *, *, #1179, .F. ) ;
#15937 = CARTESIAN_POINT ( 'NONE',  ( 56.79116909180255135, 57.79948385550240175, -4.963592699179005585 ) ) ;
#15938 = CARTESIAN_POINT ( 'NONE',  ( -154.8605857259444463, -18.79744172571344762, 15.79999999999999893 ) ) ;
#15939 = CARTESIAN_POINT ( 'NONE',  ( 55.71335778527780747, 50.09948385550240602, 1.832500667257165983 ) ) ;
#15940 = CARTESIAN_POINT ( 'NONE',  ( 75.00000000000002842, 3.000000000000000888, -5.999999999999998224 ) ) ;
#15941 = CARTESIAN_POINT ( 'NONE',  ( -4.000000000000000000, -2.309401076758512694, -5.000000000000000000 ) ) ;
#15942 = CARTESIAN_POINT ( 'NONE',  ( 45.31609314410960820, 48.30051614449765651, -6.485486291978072693 ) ) ;
#15943 = CARTESIAN_POINT ( 'NONE',  ( 51.97223112728249816, 44.60051614449766078, -5.992620115222793586 ) ) ;
#15944 = CARTESIAN_POINT ( 'NONE',  ( 6.506987859255527695, -2.925375531177290878, 5.066899051217877314 ) ) ;
#15945 = FACE_OUTER_BOUND ( 'NONE', #4881, .T. ) ;
#15946 = AXIS2_PLACEMENT_3D ( 'NONE', #18113, #4675, #16641 ) ;
#15947 = VERTEX_POINT ( 'NONE', #2615 ) ;
#15948 = AXIS2_PLACEMENT_3D ( 'NONE', #14144, #14045, #15531 ) ;
#15949 = VERTEX_POINT ( 'NONE', #11599 ) ;
#15950 = CARTESIAN_POINT ( 'NONE',  ( -1.150000000000000577, 7.225416114969384193E-16, 5.899999999999999467 ) ) ;
#15951 =( NAMED_UNIT ( * ) PLANE_ANGLE_UNIT ( ) SI_UNIT ( $, .RADIAN. ) );
#15952 = ORIENTED_EDGE ( 'NONE', *, *, #15996, .T. ) ;
#15953 = B_SPLINE_CURVE_WITH_KNOTS ( 'NONE', 3,
 ( #16053, #8875, #8588, #16439, #8780, #14756 ),
 .UNSPECIFIED., .F., .F.,
 ( 4, 2, 4 ),
 ( 0.002365888236228001588, 0.003551327329835089319, 0.004736766423442177049 ),
 .UNSPECIFIED. ) ;
#15954 = CARTESIAN_POINT ( 'NONE',  ( 43.33558569842703179, 59.09948385550240602, -2.141517661632099223 ) ) ;
#15955 = DIRECTION ( 'NONE',  ( -1.000000000000000000, 0.000000000000000000, 0.000000000000000000 ) ) ;
#15956 = COLOUR_RGB ( '',1.000000000000000000, 0.9490196078431372140, 0.9098039215686274384 ) ;
#15957 = ORIENTED_EDGE ( 'NONE', *, *, #2382, .T. ) ;
#15958 = EDGE_LOOP ( 'NONE', ( #15981, #17841, #13411, #17362 ) ) ;
#15959 = CYLINDRICAL_SURFACE ( 'NONE', #2402, 2.100000000000000089 ) ;
#15960 = ORIENTED_EDGE ( 'NONE', *, *, #15029, .F. ) ;
#15961 = CARTESIAN_POINT ( 'NONE',  ( -4.158233816355195955, -0.4370479853238878887, -9.000000000000000000 ) ) ;
#15962 = ORIENTED_EDGE ( 'NONE', *, *, #893, .T. ) ;
#15963 = CIRCLE ( 'NONE', #4064, 0.1000000000000002554 ) ;
#15964 = AXIS2_PLACEMENT_3D ( 'NONE', #15583, #5095, #18555 ) ;
#15965 = CARTESIAN_POINT ( 'NONE',  ( 44.05948171654949874, 52.79948385550240175, 4.345558710429105354 ) ) ;
#15966 = FACE_OUTER_BOUND ( 'NONE', #7116, .T. ) ;
#15967 = CARTESIAN_POINT ( 'NONE',  ( 56.65037692655921120, 49.10051614449766078, 2.184720259617097593 ) ) ;
#15968 = CYLINDRICAL_SURFACE ( 'NONE', #13618, 1.999999999999998224 ) ;
#15969 = CARTESIAN_POINT ( 'NONE',  ( -2.321707774797442170, -4.824281976789052351, -0.8000000000000000444 ) ) ;
#15970 = AXIS2_PLACEMENT_3D ( 'NONE', #11184, #8343, #6781 ) ;
#15971 = FACE_OUTER_BOUND ( 'NONE', #19082, .T. ) ;
#15972 = VERTEX_POINT ( 'NONE', #4551 ) ;
#15973 = ORIENTED_EDGE ( 'NONE', *, *, #9148, .T. ) ;
#15974 = DIRECTION ( 'NONE',  ( -1.000000000000000000, -0.000000000000000000, -0.000000000000000000 ) ) ;
#15975 = VECTOR ( 'NONE', #16446, 1000.000000000000000 ) ;
#15976 = DIRECTION ( 'NONE',  ( 0.9999419836444144449, 0.01077169184824096695, 0.000000000000000000 ) ) ;
#15977 = DIRECTION ( 'NONE',  ( -1.000000000000000000, -0.000000000000000000, -0.000000000000000000 ) ) ;
#15978 = VERTEX_POINT ( 'NONE', #10127 ) ;
#15979 = VECTOR ( 'NONE', #8585, 1000.000000000000000 ) ;
#15980 = EDGE_LOOP ( 'NONE', ( #18645, #17425 ) ) ;
#15981 = ORIENTED_EDGE ( 'NONE', *, *, #8447, .T. ) ;
#15982 = EDGE_CURVE ( 'NONE', #2647, #8711, #15322, .T. ) ;
#15983 = CARTESIAN_POINT ( 'NONE',  ( 0.000000000000000000, 0.000000000000000000, -4.974599999999998801 ) ) ;
#15984 = CARTESIAN_POINT ( 'NONE',  ( 4.082498951862917558, 4.041451884327382338, 3.558567857214853949E-17 ) ) ;
#15986 = VECTOR ( 'NONE', #10278, 1000.000000000000000 ) ;
#15985 = CARTESIAN_POINT ( 'NONE',  ( 53.50833635130544508, 51.30051614449765651, 4.867452303228181343 ) ) ;
#15987 = FACE_OUTER_BOUND ( 'NONE', #10420, .T. ) ;
#15988 = EDGE_CURVE ( 'NONE', #7251, #6069, #11240, .T. ) ;
#15989 = CARTESIAN_POINT ( 'NONE',  ( 4.104070371397480876, 2.023683613428366002, 3.505122836902507810 ) ) ;
#15990 = CARTESIAN_POINT ( 'NONE',  ( 51.92680522751233951, 53.59948385550240602, -6.007379884777223289 ) ) ;
#15991 = CIRCLE ( 'NONE', #14717, 2.649999999999985700 ) ;
#15992 = CARTESIAN_POINT ( 'NONE',  ( 0.1388410611046087539, 3.710337782248032568, 0.5735064479039790886 ) ) ;
#15993 = CONICAL_SURFACE ( 'NONE', #2849, 3.500000000000000000, 1.047197551196600296 ) ;
#15994 = CARTESIAN_POINT ( 'NONE',  ( 42.38452918213188525, 65.09948385550239891, -2.450534656007040013 ) ) ;
#15995 = CARTESIAN_POINT ( 'NONE',  ( 57.60143344285435774, 47.10051614449766078, 2.493737253992045044 ) ) ;
#15996 = EDGE_CURVE ( 'NONE', #8359, #6603, #13748, .T. ) ;
#15997 = DIRECTION ( 'NONE',  ( 0.000000000000000000, 0.000000000000000000, 1.000000000000000000 ) ) ;
#15998 = ADVANCED_FACE ( 'NONE', ( #11788 ), #8757, .T. ) ;
#15999 = CIRCLE ( 'NONE', #5664, 8.000000000000007105 ) ;
#16000 = CARTESIAN_POINT ( 'NONE',  ( -74.99999999999997158, -1.000000000000000000, 6.000000000000001776 ) ) ;
#16001 = FACE_OUTER_BOUND ( 'NONE', #16755, .T. ) ;
#16002 = EDGE_CURVE ( 'NONE', #8267, #5177, #16586, .T. ) ;
#16003 = DIRECTION ( 'NONE',  ( -1.000000000000000000, 0.000000000000000000, 6.123233995736766036E-17 ) ) ;
#16004 = EDGE_LOOP ( 'NONE', ( #16820, #8590, #6048, #4940 ) ) ;
#16005 = AXIS2_PLACEMENT_3D ( 'NONE', #5103, #6853, #18847 ) ;
#16006 = CARTESIAN_POINT ( 'NONE',  ( 0.02511973781850649831, -4.877415612947427981, -3.751298745799844792 ) ) ;
#16007 = DIRECTION ( 'NONE',  ( -0.000000000000000000, 0.000000000000000000, -1.000000000000000000 ) ) ;
#16008 = CIRCLE ( 'NONE', #350, 2.649999999999985700 ) ;
#16009 = CIRCLE ( 'NONE', #979, 3.800000000000000266 ) ;
#16010 = CARTESIAN_POINT ( 'NONE',  ( 54.13287192849671214, 52.70051614449766220, -5.649768623646139964 ) ) ;
#16011 = ADVANCED_FACE ( 'NONE', ( #4162 ), #14932, .F. ) ;
#16012 = FACE_OUTER_BOUND ( 'NONE', #17215, .T. ) ;
#16013 = EDGE_CURVE ( 'NONE', #4060, #7193, #4349, .T. ) ;
#16014 = DIRECTION ( 'NONE',  ( 1.000000000000000000, 0.000000000000000000, 0.000000000000000000 ) ) ;
#16015 = VERTEX_POINT ( 'NONE', #10417 ) ;
#16016 = FACE_OUTER_BOUND ( 'NONE', #11833, .T. ) ;
#16017 = PLANE ( 'NONE',  #3082 ) ;
#16018 = CARTESIAN_POINT ( 'NONE',  ( 49.97728705011488159, 53.49948385550240459, -7.000000000000000888 ) ) ;
#16019 = CARTESIAN_POINT ( 'NONE',  ( 0.5000000000000000000, -6.429618962271402616, 0.000000000000000000 ) ) ;
#16020 = CARTESIAN_POINT ( 'NONE',  ( 41.58830220609386430, 64.00051614449765225, -0.02388180880514929535 ) ) ;
#16021 = CARTESIAN_POINT ( 'NONE',  ( 45.86712807150329496, 49.70051614449766220, 5.649768623646139964 ) ) ;
#16022 = B_SPLINE_CURVE_WITH_KNOTS ( 'NONE', 3,
 ( #2688, #12767, #2393, #14324, #16108, #906 ),
 .UNSPECIFIED., .F., .F.,
 ( 4, 2, 4 ),
 ( 0.002452478801916361129, 0.003676905084148001344, 0.004901331366379641126 ),
 .UNSPECIFIED. ) ;
#16023 = CARTESIAN_POINT ( 'NONE',  ( -2.321707774797442170, -4.824281976789052351, -0.8000000000000000444 ) ) ;
#16024 = CARTESIAN_POINT ( 'NONE',  ( 6.362382503762741948, -2.018850626433581041, 5.108861885121540602 ) ) ;
#16025 = AXIS2_PLACEMENT_3D ( 'NONE', #7060, #14311, #2674 ) ;
#16026 = ORIENTED_EDGE ( 'NONE', *, *, #16256, .T. ) ;
#16027 = TOROIDAL_SURFACE ( 'NONE', #11944, 3.299999999999999822, 0.2000000000000000111 ) ;
#16028 = ORIENTED_EDGE ( 'NONE', *, *, #1273, .T. ) ;
#16029 = DIRECTION ( 'NONE',  ( 1.000000000000000000, 0.000000000000000000, 0.000000000000000000 ) ) ;
#16030 = VERTEX_POINT ( 'NONE', #10316 ) ;
#16031 = CARTESIAN_POINT ( 'NONE',  ( 2.449293598294706513E-15, -20.00000000000000000, 9.000000000000000000 ) ) ;
#16032 = EDGE_LOOP ( 'NONE', ( #5092, #12810, #2551, #1072, #14197, #17021, #1844, #18401, #727, #13058, #3646, #5796, #10851, #3668, #1077, #7974, #4488, #17488, #8903, #4945, #9745, #13217, #6413, #9643, #13155, #10128, #8861, #8179, #3290, #11454, #15740, #11520, #12956, #1280, #17951, #5113, #6258, #10354, #16472, #11842, #13311, #11104, #17025, #8242, #5387, #922, #2729, #14350, #11306, #14246, #179, #9618, #7113, #388, #4889, #18937, #15434, #14249, #1456, #17408, #13121, #7406, #2924, #15054, #15412, #9633, #13132, #9733, #5947, #10681, #19257, #2612, #6028, #17613, #13608 ) ) ;
#16033 = DIRECTION ( 'NONE',  ( 0.000000000000000000, 0.000000000000000000, 1.000000000000000000 ) ) ;
#16034 = ORIENTED_EDGE ( 'NONE', *, *, #12148, .T. ) ;
#16035 = EDGE_CURVE ( 'NONE', #13101, #514, #17699, .T. ) ;
#16036 = DIRECTION ( 'NONE',  ( -0.000000000000000000, -0.000000000000000000, 1.000000000000000000 ) ) ;
#16037 = ORIENTED_EDGE ( 'NONE', *, *, #6152, .T. ) ;
#16038 = CARTESIAN_POINT ( 'NONE',  ( 47.42335538002188144, 58.59948385550239891, 8.007379884777233059 ) ) ;
#16039 = CARTESIAN_POINT ( 'NONE',  ( 1.398397006336996817, -6.091550361990593743, -0.8000000000000000444 ) ) ;
#16040 = PRODUCT_DEFINITION_SHAPE ( 'NONE', 'NONE',  #19438 ) ;
#16041 = CARTESIAN_POINT ( 'NONE',  ( 44.88205777487398507, 49.19948385550240744, -3.688883143319540814 ) ) ;
#16042 = EDGE_CURVE ( 'NONE', #11631, #17511, #4979, .T. ) ;
#16043 = CARTESIAN_POINT ( 'NONE',  ( 2.449293598294706513E-15, -20.00000000000000000, 15.00000000000000355 ) ) ;
#16044 = VECTOR ( 'NONE', #5760, 1000.000000000000000 ) ;
#16045 = CARTESIAN_POINT ( 'NONE',  ( 25.00000000000000711, -20.00000000000000000, -20.00000000000000000 ) ) ;
#16046 = CARTESIAN_POINT ( 'NONE',  ( 43.18075615816994173, 45.80051614449766362, 4.924951120819380357 ) ) ;
#16047 = CARTESIAN_POINT ( 'NONE',  ( 56.30877334542961421, 47.00051614449766646, 0.02388180880515774693 ) ) ;
#16048 = CARTESIAN_POINT ( 'NONE',  ( 1.391697335622810172, 4.043246145443375461, -3.503898532754365913 ) ) ;
#16049 = DIRECTION ( 'NONE',  ( 0.000000000000000000, 0.000000000000000000, 1.000000000000000000 ) ) ;
#16050 = EDGE_LOOP ( 'NONE', ( #4181, #1508, #7606, #10728 ) ) ;
#16051 = AXIS2_PLACEMENT_3D ( 'NONE', #17806, #4661, #7781 ) ;
#16052 = ORIENTED_EDGE ( 'NONE', *, *, #15282, .F. ) ;
#16053 = CARTESIAN_POINT ( 'NONE',  ( -2.000000000000007550, -3.464101615137749945, 0.000000000000000000 ) ) ;
#16054 = ORIENTED_EDGE ( 'NONE', *, *, #8002, .T. ) ;
#16055 = EDGE_CURVE ( 'NONE', #4604, #16860, #2795, .T. ) ;
#16056 = CARTESIAN_POINT ( 'NONE',  ( 52.25172492374522903, 59.59948385550240602, -7.007379884777225953 ) ) ;
#16057 = FACE_OUTER_BOUND ( 'NONE', #11436, .T. ) ;
#16058 = ORIENTED_EDGE ( 'NONE', *, *, #4420, .T. ) ;
#16059 = EDGE_LOOP ( 'NONE', ( #781, #13092, #134, #13863, #8495 ) ) ;
#16060 = CARTESIAN_POINT ( 'NONE',  ( -52.34999999999998010, -14.99999999999998579, 15.00000000000000000 ) ) ;
#16061 = EDGE_CURVE ( 'NONE', #9398, #965, #7192, .T. ) ;
#16062 = DIRECTION ( 'NONE',  ( -3.469446951953614682E-16, 1.000000000000000000, 0.000000000000000000 ) ) ;
#16063 = ORIENTED_EDGE ( 'NONE', *, *, #14592, .F. ) ;
#16064 = CYLINDRICAL_SURFACE ( 'NONE', #10677, 2.649999999999985700 ) ;
#16065 = ORIENTED_EDGE ( 'NONE', *, *, #892, .T. ) ;
#16066 = LINE ( 'NONE', #11725, #8203 ) ;
#16067 = CARTESIAN_POINT ( 'NONE',  ( 52.25172492374522903, 51.59948385550240602, -7.007379884777225953 ) ) ;
#16068 = DIRECTION ( 'NONE',  ( -1.000000000000000000, 0.000000000000000000, 0.000000000000000000 ) ) ;
#16069 = CARTESIAN_POINT ( 'NONE',  ( 45.86712807150329496, 47.70051614449766220, 5.649768623646139964 ) ) ;
#16070 = CARTESIAN_POINT ( 'NONE',  ( -20.00000000000000000, -19.99999999999999289, -20.00000000000000000 ) ) ;
#16071 = CARTESIAN_POINT ( 'NONE',  ( 2.000000000000000000, -1.773042676681341856, 2.276824562219559311E-15 ) ) ;
#16072 = PRODUCT_DEFINITION_FORMATION_WITH_SPECIFIED_SOURCE ( 'ANY', '', #13052, .NOT_KNOWN. ) ;
#16073 = CARTESIAN_POINT ( 'NONE',  ( 30.00000000000000000, -3.000000000000002665, -5.999999999999998224 ) ) ;
#16074 =( BOUNDED_SURFACE ( )  B_SPLINE_SURFACE ( 3, 2, ( 
 ( #8526, #1078, #11649 ),
 ( #18845, #13128, #13029 ),
 ( #4209, #10176, #11358 ),
 ( #17363, #3924, #16176 ),
 ( #15882, #4116, #2756 ),
 ( #8712, #984, #7048 ) ),
 .UNSPECIFIED., .F., .F., .T. ) 
 B_SPLINE_SURFACE_WITH_KNOTS ( ( 4, 2, 4 ),
 ( 3, 3 ),
 ( 0.02367865728600889244, 0.02663179453327095547, 0.02958493178053301503 ),
 ( 0.000000000000000000, 1.000000000000000000 ),
 .UNSPECIFIED. ) 
 GEOMETRIC_REPRESENTATION_ITEM ( )  RATIONAL_B_SPLINE_SURFACE ( (
 ( 1.000000000000000000, 0.8047781103519378032, 1.000000000000000000),
 ( 1.000000000000000000, 0.8123785825977077879, 1.000000000000000000),
 ( 1.000000000000000000, 0.8190671539292031511, 1.000000000000000000),
 ( 1.000000000000000000, 0.8192352255331103450, 1.000000000000000000),
 ( 1.000000000000000000, 0.8126129676838903526, 1.000000000000000000),
 ( 1.000000000000000000, 0.8047712537969723412, 1.000000000000000000) ) ) 
 REPRESENTATION_ITEM ( '' )  SURFACE ( )  );
#16075 = ORIENTED_EDGE ( 'NONE', *, *, #15190, .T. ) ;
#16076 = ORIENTED_EDGE ( 'NONE', *, *, #1782, .F. ) ;
#16077 = CARTESIAN_POINT ( 'NONE',  ( 0.9183817310753817909, -24.91493387504115020, 9.999999999999998224 ) ) ;
#16078 = FILL_AREA_STYLE ('',( #19330 ) ) ;
#16079 = CARTESIAN_POINT ( 'NONE',  ( -2.649999999999988365, 15.00000000000001599, -9.999999999999998224 ) ) ;
#16080 = FILL_AREA_STYLE ('',( #17557 ) ) ;
#16081 = ORIENTED_EDGE ( 'NONE', *, *, #12958, .F. ) ;
#16082 = CARTESIAN_POINT ( 'NONE',  ( -150.9999999999999716, -14.99999999999999645, 6.499999999999999112 ) ) ;
#16083 = ORIENTED_EDGE ( 'NONE', *, *, #10462, .T. ) ;
#16084 = ORIENTED_EDGE ( 'NONE', *, *, #10234, .F. ) ;
#16085 = CARTESIAN_POINT ( 'NONE',  ( 4.799999999999999822, 0.000000000000000000, -1.000000000000000000 ) ) ;
#16086 = CARTESIAN_POINT ( 'NONE',  ( 4.175075985190098038, 4.120741555260245548, 3.964526709274768569E-16 ) ) ;
#16087 = CARTESIAN_POINT ( 'NONE',  ( 46.45491332379576477, 47.70051614449766220, 4.840751629271188961 ) ) ;
#16088 = LINE ( 'NONE', #1086, #13605 ) ;
#16089 = LINE ( 'NONE', #12749, #8688 ) ;
#16090 = CARTESIAN_POINT ( 'NONE',  ( 56.30877334542961421, 53.99948385550241170, -0.02388180880520959434 ) ) ;
#16091 = FACE_OUTER_BOUND ( 'NONE', #15834, .T. ) ;
#16092 = CARTESIAN_POINT ( 'NONE',  ( 45.31609314410967926, 64.69948385550240744, 6.485486291978119766 ) ) ;
#16093 = CARTESIAN_POINT ( 'NONE',  ( 43.18075615816994173, 45.80051614449766362, 4.924951120819380357 ) ) ;
#16094 = CARTESIAN_POINT ( 'NONE',  ( 0.3106000600989247684, -3.122278952918441597, 4.592054218142290978 ) ) ;
#16095 = CARTESIAN_POINT ( 'NONE',  ( 7.336184427528458230, 0.000000000000000000, 0.000000000000000000 ) ) ;
#16096 = FILL_AREA_STYLE ('',( #14809 ) ) ;
#16097 = ADVANCED_FACE ( 'NONE', ( #11987 ), #11550, .T. ) ;
#16098 = SHAPE_DEFINITION_REPRESENTATION ( #5707, #10550 ) ;
#16099 = VERTEX_POINT ( 'NONE', #2896 ) ;
#16100 = PRODUCT_RELATED_PRODUCT_CATEGORY ( 'part', '', ( #12728 ) ) ;
#16101 = CARTESIAN_POINT ( 'NONE',  ( -4.175002511812151873, -2.208363329454905877, -3.469254087858246738 ) ) ;
#16102 = AXIS2_PLACEMENT_3D ( 'NONE', #4464, #4657, #14940 ) ;
#16103 = CARTESIAN_POINT ( 'NONE',  ( 7.211304515372821022, -38.65468003441933575, 0.000000000000000000 ) ) ;
#16104 = VECTOR ( 'NONE', #15619, 1000.000000000000000 ) ;
#16105 = ADVANCED_FACE ( 'NONE', ( #19283, #8858, #17991, #5921 ), #14536, .F. ) ;
#16106 = ADVANCED_FACE ( 'NONE', ( #14630 ), #11885, .T. ) ;
#16107 = CARTESIAN_POINT ( 'NONE',  ( 2.449293598294706513E-15, -20.00000000000000000, -20.00000000000000000 ) ) ;
#16108 = CARTESIAN_POINT ( 'NONE',  ( 4.207491450040567571, -2.029819825146485179, -3.671670828759567407 ) ) ;
#16109 = CARTESIAN_POINT ( 'NONE',  ( -154.9999999999999716, -14.99999999999999645, -15.79999999999999893 ) ) ;
#16110 = FACE_BOUND ( 'NONE', #13654, .T. ) ;
#16111 = EDGE_CURVE ( 'NONE', #12615, #10736, #1271, .T. ) ;
#16112 = CARTESIAN_POINT ( 'NONE',  ( 1.925929944387235853E-31, 15.00000000000001599, 9.000000000000000000 ) ) ;
#16113 = CARTESIAN_POINT ( 'NONE',  ( 52.25172492374522903, 49.59948385550240602, -7.007379884777225953 ) ) ;
#16114 = EDGE_CURVE ( 'NONE', #5403, #18909, #11565, .T. ) ;
#16115 = CARTESIAN_POINT ( 'NONE',  ( -17.32050807568872841, -30.00000000000008171, -9.000000000000000000 ) ) ;
#16116 = CARTESIAN_POINT ( 'NONE',  ( 58.41169779390614281, 49.99948385550240459, -0.02388180880523160798 ) ) ;
#16117 = CARTESIAN_POINT ( 'NONE',  ( 45.90387839640208512, 48.30051614449765651, -5.676469297603124353 ) ) ;
#16118 = CARTESIAN_POINT ( 'NONE',  ( 0.000000000000000000, 0.000000000000000000, 0.000000000000000000 ) ) ;
#16119 = CIRCLE ( 'NONE', #8260, 5.000000000000000888 ) ;
#16121 = VERTEX_POINT ( 'NONE', #1898 ) ;
#16120 = EDGE_CURVE ( 'NONE', #9930, #730, #330, .T. ) ;
#16122 = EDGE_CURVE ( 'NONE', #13131, #1122, #5021, .T. ) ;
#16123 = ORIENTED_EDGE ( 'NONE', *, *, #7171, .T. ) ;
#16124 = DIRECTION ( 'NONE',  ( -1.000000000000000000, -0.000000000000000000, -0.000000000000000000 ) ) ;
#16125 = ORIENTED_EDGE ( 'NONE', *, *, #3537, .T. ) ;
#16126 = DIRECTION ( 'NONE',  ( -1.000000000000000000, -0.000000000000000000, -0.000000000000000000 ) ) ;
#16127 = ORIENTED_EDGE ( 'NONE', *, *, #8421, .T. ) ;
#16128 = FACE_BOUND ( 'NONE', #5335, .T. ) ;
#16129 = EDGE_CURVE ( 'NONE', #6347, #8396, #16513, .T. ) ;
#16130 = ORIENTED_EDGE ( 'NONE', *, *, #9544, .F. ) ;
#16131 = AXIS2_PLACEMENT_3D ( 'NONE', #3352, #15490, #3258 ) ;
#16132 = EDGE_CURVE ( 'NONE', #10976, #71, #16800, .T. ) ;
#16133 = DIRECTION ( 'NONE',  ( 0.000000000000000000, 0.000000000000000000, 1.000000000000000000 ) ) ;
#16134 = ORIENTED_EDGE ( 'NONE', *, *, #18774, .T. ) ;
#16135 = CARTESIAN_POINT ( 'NONE',  ( 41.58830220609386430, 58.99948385550239749, 0.02388180880523263147 ) ) ;
#16136 = AXIS2_PLACEMENT_3D ( 'NONE', #8914, #7349, #3048 ) ;
#16137 = CARTESIAN_POINT ( 'NONE',  ( -14.17539641854911459, -34.10879641843998655, 9.000000000000000000 ) ) ;
#16138 = CARTESIAN_POINT ( 'NONE',  ( 53.50833635130540955, 53.69948385550240744, -4.867452303228209765 ) ) ;
#16139 = EDGE_CURVE ( 'NONE', #6054, #14216, #10391, .T. ) ;
#16140 = CARTESIAN_POINT ( 'NONE',  ( 2.449293598294706513E-15, -20.00000000000000000, -9.000000000000000000 ) ) ;
#16141 = DIRECTION ( 'NONE',  ( 0.000000000000000000, -0.5000000000000004441, 0.8660254037844383745 ) ) ;
#16142 = CARTESIAN_POINT ( 'NONE',  ( 54.72065718078918906, 44.70051614449765509, -6.458785618021089192 ) ) ;
#16143 = CIRCLE ( 'NONE', #1101, 0.9999999999999991118 ) ;
#16144 = CARTESIAN_POINT ( 'NONE',  ( 49.97728705011494554, 47.50051614449765935, 6.000000000000000888 ) ) ;
#16145 = DIRECTION ( 'NONE',  ( 1.000000000000000000, 0.000000000000000000, 0.000000000000000000 ) ) ;
#16146 = DIRECTION ( 'NONE',  ( 1.000000000000000000, 0.000000000000000000, 0.000000000000000000 ) ) ;
#16147 = ORIENTED_EDGE ( 'NONE', *, *, #10319, .F. ) ;
#16148 = ORIENTED_EDGE ( 'NONE', *, *, #9249, .F. ) ;
#16149 = DIRECTION ( 'NONE',  ( 0.000000000000000000, 0.000000000000000000, -1.000000000000000000 ) ) ;
#16150 = EDGE_LOOP ( 'NONE', ( #14398, #4281, #5045, #16153 ) ) ;
#16151 = CARTESIAN_POINT ( 'NONE',  ( 47.74827507625478518, 58.59948385550238470, 7.007379884777227730 ) ) ;
#16152 = CARTESIAN_POINT ( 'NONE',  ( -20.00000000000000000, -25.00000000000000000, -23.00000000000000000 ) ) ;
#16153 = ORIENTED_EDGE ( 'NONE', *, *, #10456, .T. ) ;
#16154 = EDGE_LOOP ( 'NONE', ( #18884, #16367, #11782, #5608, #19016, #12133, #14739, #15540, #4999, #533 ) ) ;
#16155 = DIRECTION ( 'NONE',  ( 0.000000000000000000, 0.000000000000000000, 1.000000000000000000 ) ) ;
#16156 = AXIS2_PLACEMENT_3D ( 'NONE', #1299, #17672, #3943 ) ;
#16157 = CARTESIAN_POINT ( 'NONE',  ( -72.99999999999997158, 2.999999999999999112, -5.999999999999998224 ) ) ;
#16158 = VERTEX_POINT ( 'NONE', #18190 ) ;
#16159 = DIRECTION ( 'NONE',  ( 0.000000000000000000, 0.000000000000000000, -1.000000000000000000 ) ) ;
#16160 = ORIENTED_EDGE ( 'NONE', *, *, #18778, .T. ) ;
#16161 = DIRECTION ( 'NONE',  ( 1.000000000000000000, 0.000000000000000000, 0.000000000000000000 ) ) ;
#16162 = CARTESIAN_POINT ( 'NONE',  ( 42.63976443033212860, 48.99948385550240459, 0.02388180880522514787 ) ) ;
#16163 = CARTESIAN_POINT ( 'NONE',  ( 6.080745460913608902, 0.5192545390863916310, -1.000000000000000000 ) ) ;
#16164 = CARTESIAN_POINT ( 'NONE',  ( 44.03140696652198471, 47.80051614449764230, 4.306917132069485454 ) ) ;
#16165 = CARTESIAN_POINT ( 'NONE',  ( 0.000000000000000000, 0.000000000000000000, 0.000000000000000000 ) ) ;
#16166 = EDGE_CURVE ( 'NONE', #10751, #11229, #13887, .T. ) ;
#16167 = DIRECTION ( 'NONE',  ( 0.01780247661957949992, 0.9998415233556812165, -7.576222706442768103E-17 ) ) ;
#16168 = AXIS2_PLACEMENT_3D ( 'NONE', #13886, #5265, #11236 ) ;
#16169 = EDGE_CURVE ( 'NONE', #10416, #6867, #1615, .T. ) ;
#16170 = ORIENTED_EDGE ( 'NONE', *, *, #3832, .T. ) ;
#16171 = VERTEX_POINT ( 'NONE', #9231 ) ;
#16172 = DIRECTION ( 'NONE',  ( 0.000000000000000000, 0.000000000000000000, 1.000000000000000000 ) ) ;
#16173 = CARTESIAN_POINT ( 'NONE',  ( 0.000000000000000000, 0.000000000000000000, -10.00000000000000000 ) ) ;
#16174 = DIRECTION ( 'NONE',  ( 2.191393683118473446E-17, 7.538405132783725260E-17, 1.000000000000000000 ) ) ;
#16175 = EDGE_LOOP ( 'NONE', ( #8409, #8965, #8052, #12015 ) ) ;
#16176 = CARTESIAN_POINT ( 'NONE',  ( 6.242800618755108388, 4.918813924286816963, 1.690830708135752758 ) ) ;
#16177 = ORIENTED_EDGE ( 'NONE', *, *, #3759, .T. ) ;
#16178 = ORIENTED_EDGE ( 'NONE', *, *, #2341, .T. ) ;
#16179 = DIRECTION ( 'NONE',  ( 0.000000000000000000, 0.000000000000000000, 1.000000000000000000 ) ) ;
#16180 = UNCERTAINTY_MEASURE_WITH_UNIT (LENGTH_MEASURE( 1.000000000000000082E-05 ), #2564, 'distance_accuracy_value', 'NONE');
#16181 = CARTESIAN_POINT ( 'NONE',  ( 48.02776887271750184, 47.60051614449766078, 5.992620115222795363 ) ) ;
#16182 = CARTESIAN_POINT ( 'NONE',  ( 0.01055556052339245120, -4.575665857285984295, -2.074714256722479888 ) ) ;
#16183 = CARTESIAN_POINT ( 'NONE',  ( -14.86289650954790886, -6.617387872822862782, -9.000000000000000000 ) ) ;
#16184 = CARTESIAN_POINT ( 'NONE',  ( 46.45491332379572924, 49.29948385550240886, -4.840751629271157874 ) ) ;
#16185 = CARTESIAN_POINT ( 'NONE',  ( -22.14999999999999858, -19.99999999999999289, -20.00000000000000000 ) ) ;
#16186 = CARTESIAN_POINT ( 'NONE',  ( 54.13287192849676188, 54.29948385550240886, 5.649768623646098220 ) ) ;
#16187 = CARTESIAN_POINT ( 'NONE',  ( 47.37792948025170858, 49.60051614449766788, 7.992620115222797139 ) ) ;
#16188 = CARTESIAN_POINT ( 'NONE',  ( -4.000000000000000000, -2.309401076758512694, -3.433295621305382461 ) ) ;
#16189 = AXIS2_PLACEMENT_3D ( 'NONE', #13932, #9332, #513 ) ;
#16190 = DIRECTION ( 'NONE',  ( 0.000000000000000000, 0.000000000000000000, 1.000000000000000000 ) ) ;
#16191 = DIRECTION ( 'NONE',  ( 1.000000000000000000, 0.000000000000000000, 0.000000000000000000 ) ) ;
#16192 = AXIS2_PLACEMENT_3D ( 'NONE', #716, #3753, #9719 ) ;
#16193 = VERTEX_POINT ( 'NONE', #7578 ) ;
#16194 = CARTESIAN_POINT ( 'NONE',  ( -0.5449313310646672903, -4.304185902836978883, -3.316620875263469159 ) ) ;
#16195 = CLOSED_SHELL ( 'NONE', ( #8905, #12022, #15509, #17720, #7239, #7057 ) ) ;
#16196 = DIRECTION ( 'NONE',  ( -0.000000000000000000, 0.000000000000000000, 1.000000000000000000 ) ) ;
#16197 = AXIS2_PLACEMENT_3D ( 'NONE', #17388, #14224, #15811 ) ;
#16198 = CARTESIAN_POINT ( 'NONE',  ( -2.805705207896067144, 3.226868319750155312, -3.503898532754364581 ) ) ;
#16199 = LINE ( 'NONE', #17773, #4631 ) ;
#16200 = ADVANCED_BREP_SHAPE_REPRESENTATION ( '', ( #15430, #10359 ), #12782 ) ;
#16201 = DIRECTION ( 'NONE',  ( 0.000000000000000000, 0.000000000000000000, 1.000000000000000000 ) ) ;
#16202 = AXIS2_PLACEMENT_3D ( 'NONE', #18435, #10955, #3145 ) ;
#16203 = LINE ( 'NONE', #13060, #8896 ) ;
#16204 = EDGE_CURVE ( 'NONE', #9645, #3228, #7819, .T. ) ;
#16205 = CARTESIAN_POINT ( 'NONE',  ( -0.1756481739660520902, 4.720212674038980261, -3.469390959564065291 ) ) ;
#16206 = CARTESIAN_POINT ( 'NONE',  ( 47.74827507625478518, 50.59948385550238470, 7.007379884777227730 ) ) ;
#16207 = DIRECTION ( 'NONE',  ( 0.000000000000000000, -0.000000000000000000, 1.000000000000000000 ) ) ;
#16208 = CARTESIAN_POINT ( 'NONE',  ( 57.61547081786812896, 54.09948385550241312, 2.450534656007040901 ) ) ;
#16209 = CARTESIAN_POINT ( 'NONE',  ( 2.000000000000000000, -0.8865213383406694847, 1.535500000000001419 ) ) ;
#16210 = CARTESIAN_POINT ( 'NONE',  ( 43.34962307344078880, 50.10051614449766078, -2.184720259617096705 ) ) ;
#16211 = CIRCLE ( 'NONE', #16527, 2.447112362156698140 ) ;
#16212 = CARTESIAN_POINT ( 'NONE',  ( 50.00000000000000000, 15.00000000000000000, 0.000000000000000000 ) ) ;
#16213 = ORIENTED_EDGE ( 'NONE', *, *, #1257, .T. ) ;
#16214 = CIRCLE ( 'NONE', #11821, 5.000000000000000888 ) ;
#16215 = VERTEX_POINT ( 'NONE', #6309 ) ;
#16216 = FACE_OUTER_BOUND ( 'NONE', #12101, .T. ) ;
#16217 = AXIS2_PLACEMENT_3D ( 'NONE', #5149, #840, #12699 ) ;
#16218 = ORIENTED_EDGE ( 'NONE', *, *, #9868, .T. ) ;
#16219 = CARTESIAN_POINT ( 'NONE',  ( -4.158233816355060064, -39.56295201467614220, -9.000000000000000000 ) ) ;
#16220 = EDGE_CURVE ( 'NONE', #8101, #1464, #9996, .T. ) ;
#16221 = VERTEX_POINT ( 'NONE', #4834 ) ;
#16222 = LINE ( 'NONE', #17701, #14731 ) ;
#16223 = ORIENTED_EDGE ( 'NONE', *, *, #7372, .F. ) ;
#16224 = CARTESIAN_POINT ( 'NONE',  ( 1.250000000000000000, -6.429618962271402616, 0.000000000000000000 ) ) ;
#16225 = ORIENTED_EDGE ( 'NONE', *, *, #7858, .F. ) ;
#16226 = VECTOR ( 'NONE', #3475, 1000.000000000000000 ) ;
#16227 = CARTESIAN_POINT ( 'NONE',  ( 56.81924384183011512, 62.19948385550240744, 4.924951120819313743 ) ) ;
#16228 = DIRECTION ( 'NONE',  ( -1.000000000000000000, 0.000000000000000000, 0.000000000000000000 ) ) ;
#16229 = ADVANCED_FACE ( 'NONE', ( #7957 ), #13927, .F. ) ;
#16230 = AXIS2_PLACEMENT_3D ( 'NONE', #15799, #2380, #8334 ) ;
#16231 = CARTESIAN_POINT ( 'NONE',  ( 48.02776887271745210, 55.39948385550240317, -5.992620115222778487 ) ) ;
#16233 = EDGE_CURVE ( 'NONE', #6154, #14289, #11563, .T. ) ;
#16232 = FACE_OUTER_BOUND ( 'NONE', #19411, .T. ) ;
#16234 = CARTESIAN_POINT ( 'NONE',  ( 1.171083334267915221, -24.65495046420793201, 9.999999999999998224 ) ) ;
#16235 = CARTESIAN_POINT ( 'NONE',  ( 54.68390685589039890, 47.30051614449766362, 6.485486291978072693 ) ) ;
#16236 = CARTESIAN_POINT ( 'NONE',  ( 46.45491332379576477, 51.70051614449765509, 4.840751629271188961 ) ) ;
#16237 = EDGE_CURVE ( 'NONE', #4109, #1031, #9711, .T. ) ;
#16238 = DIRECTION ( 'NONE',  ( 1.000000000000000000, 0.000000000000000000, 0.000000000000000000 ) ) ;
#16239 = ORIENTED_EDGE ( 'NONE', *, *, #6157, .F. ) ;
#16240 = ADVANCED_FACE ( 'NONE', ( #12951 ), #5207, .T. ) ;
#16241 = ORIENTED_EDGE ( 'NONE', *, *, #17684, .T. ) ;
#16242 = DIRECTION ( 'NONE',  ( -1.000000000000000000, -0.000000000000000000, -0.000000000000000000 ) ) ;
#16243 = VERTEX_POINT ( 'NONE', #17187 ) ;
#16244 = VECTOR ( 'NONE', #2662, 1000.000000000000114 ) ;
#16245 = VECTOR ( 'NONE', #16172, 1000.000000000000000 ) ;
#16246 = CARTESIAN_POINT ( 'NONE',  ( 4.158233816354936607, -0.4370479853238358192, -9.000000000000000000 ) ) ;
#16247 = ORIENTED_EDGE ( 'NONE', *, *, #7302, .T. ) ;
#16248 = ORIENTED_EDGE ( 'NONE', *, *, #18280, .T. ) ;
#16249 = CARTESIAN_POINT ( 'NONE',  ( -1.000000000000000222, -4.808326913195983821, -0.8000000000000000444 ) ) ;
#16250 = CARTESIAN_POINT ( 'NONE',  ( 57.36023556966787851, 45.99948385550239749, -0.02388180880522424582 ) ) ;
#16251 = ORIENTED_EDGE ( 'NONE', *, *, #14235, .F. ) ;
#16252 = MECHANICAL_DESIGN_GEOMETRIC_PRESENTATION_REPRESENTATION (  '', ( #14359 ), #5915 ) ;
#16253 = DIRECTION ( 'NONE',  ( -0.000000000000000000, -0.000000000000000000, 1.000000000000000000 ) ) ;
#16254 = VERTEX_POINT ( 'NONE', #14023 ) ;
#16255 = DIRECTION ( 'NONE',  ( 0.000000000000000000, 0.000000000000000000, 1.000000000000000000 ) ) ;
#16256 = EDGE_CURVE ( 'NONE', #6411, #5143, #805, .T. ) ;
#16257 = CARTESIAN_POINT ( 'NONE',  ( 52.29715082351547295, 54.39948385550239607, 6.992620115222774047 ) ) ;
#16258 = EDGE_CURVE ( 'NONE', #2267, #18916, #12859, .T. ) ;
#16259 = FACE_OUTER_BOUND ( 'NONE', #16004, .T. ) ;
#16260 = CARTESIAN_POINT ( 'NONE',  ( 49.97728705011495265, 47.50051614449766646, 7.000000000000000888 ) ) ;
#16261 = CARTESIAN_POINT ( 'NONE',  ( 3.951447005078451813, -1.347150628109131443, -3.500000000000000444 ) ) ;
#16262 = MECHANICAL_DESIGN_GEOMETRIC_PRESENTATION_REPRESENTATION (  '', ( #8732 ), #1532 ) ;
#16263 = VECTOR ( 'NONE', #6348, 1000.000000000000000 ) ;
#16264 = CARTESIAN_POINT ( 'NONE',  ( 13.99999999999999822, 0.000000000000000000, 1.610000000000000098 ) ) ;
#16265 = CARTESIAN_POINT ( 'NONE',  ( 2.000000000000000000, 1.773042676681340524, -2.059984127722458425E-15 ) ) ;
#16266 = AXIS2_PLACEMENT_3D ( 'NONE', #9707, #14418, #12757 ) ;
#16267 = ORIENTED_EDGE ( 'NONE', *, *, #5778, .T. ) ;
#16268 = VERTEX_POINT ( 'NONE', #8149 ) ;
#16269 = FACE_BOUND ( 'NONE', #11314, .T. ) ;
#16270 =( LENGTH_UNIT ( ) NAMED_UNIT ( * ) SI_UNIT ( .MILLI., .METRE. ) );
#16271 = CARTESIAN_POINT ( 'NONE',  ( 50.02271294988512551, 46.49948385550240459, 7.000000000000000888 ) ) ;
#16272 = DIRECTION ( 'NONE',  ( -0.000000000000000000, -0.000000000000000000, 1.000000000000000000 ) ) ;
#16273 = VERTEX_POINT ( 'NONE', #2187 ) ;
#16274 = B_SPLINE_CURVE_WITH_KNOTS ( 'NONE', 3,
 ( #4419, #9009, #16182, #2762, #13323, #14696, #16286, #4517 ),
 .UNSPECIFIED., .F., .F.,
 ( 4, 2, 2, 4 ),
 ( 0.002921158011986710323, 0.003648658599403064445, 0.004376159186819419435, 0.005831160361652128546 ),
 .UNSPECIFIED. ) ;
#16275 = DIRECTION ( 'NONE',  ( 0.000000000000000000, 0.000000000000000000, 1.000000000000000000 ) ) ;
#16276 = AXIS2_PLACEMENT_3D ( 'NONE', #10030, #9829, #14049 ) ;
#16277 = AXIS2_PLACEMENT_3D ( 'NONE', #2915, #10242, #5747 ) ;
#16278 = VERTEX_POINT ( 'NONE', #17291 ) ;
#16279 = ORIENTED_EDGE ( 'NONE', *, *, #3415, .F. ) ;
#16280 = EDGE_CURVE ( 'NONE', #4855, #13890, #10932, .T. ) ;
#16281 = CYLINDRICAL_SURFACE ( 'NONE', #5989, 1.000000000000000888 ) ;
#16282 = DIRECTION ( 'NONE',  ( 0.000000000000000000, 0.000000000000000000, -1.000000000000000000 ) ) ;
#16283 = AXIS2_PLACEMENT_3D ( 'NONE', #11857, #4428, #19052 ) ;
#16284 = ADVANCED_FACE ( 'NONE', ( #3848 ), #10626, .T. ) ;
#16285 = CARTESIAN_POINT ( 'NONE',  ( 49.97728705011494554, 49.50051614449766646, 6.000000000000000888 ) ) ;
#16286 = CARTESIAN_POINT ( 'NONE',  ( 0.3106000600989309857, -5.537975084925943037, -0.4079457818577079120 ) ) ;
#16287 = EDGE_CURVE ( 'NONE', #12831, #10827, #3748, .T. ) ;
#16288 = SURFACE_STYLE_FILL_AREA ( #6176 ) ;
#16289 = CARTESIAN_POINT ( 'NONE',  ( 50.02271294988511841, 60.49948385550240459, 6.000000000000000888 ) ) ;
#16290 = CARTESIAN_POINT ( 'NONE',  ( 10.00000000000000000, 15.00000000000001776, -15.00000000000000000 ) ) ;
#16291 = CARTESIAN_POINT ( 'NONE',  ( 47.70284917648453415, 51.39948385550238896, -6.992620115222774047 ) ) ;
#16292 = AXIS2_PLACEMENT_3D ( 'NONE', #16301, #8544, #1487 ) ;
#16293 = CARTESIAN_POINT ( 'NONE',  ( 47.42335538002180328, 48.40051614449766504, -8.007379884777206414 ) ) ;
#16294 = FACE_OUTER_BOUND ( 'NONE', #1439, .T. ) ;
#16295 = DIRECTION ( 'NONE',  ( 1.000000000000000000, 0.000000000000000000, 0.000000000000000000 ) ) ;
#16296 = CARTESIAN_POINT ( 'NONE',  ( 0.000000000000000000, 0.000000000000000000, 0.000000000000000000 ) ) ;
#16297 = AXIS2_PLACEMENT_3D ( 'NONE', #5941, #10335, #16339 ) ;
#16298 = ORIENTED_EDGE ( 'NONE', *, *, #7039, .F. ) ;
#16299 = DIRECTION ( 'NONE',  ( -1.000000000000000000, 0.000000000000000000, 0.000000000000000000 ) ) ;
#16300 = ADVANCED_FACE ( 'NONE', ( #9808, #6583 ), #6778, .F. ) ;
#16301 = CARTESIAN_POINT ( 'NONE',  ( 1.925929944387235853E-31, 15.00000000000001599, 15.00000000000000178 ) ) ;
#16302 = AXIS2_PLACEMENT_3D ( 'NONE', #9023, #15011, #13545 ) ;
#16303 = ADVANCED_FACE ( 'NONE', ( #6871 ), #711, .T. ) ;
#16304 = DIRECTION ( 'NONE',  ( 1.000000000000000000, 0.000000000000000000, 0.000000000000000000 ) ) ;
#16305 = CARTESIAN_POINT ( 'NONE',  ( 5.991014884144048480, 4.330127018922193649, 2.500000000000001776 ) ) ;
#16306 = AXIS2_PLACEMENT_3D ( 'NONE', #19125, #11639, #1068 ) ;
#16307 = DIRECTION ( 'NONE',  ( 0.000000000000000000, 0.000000000000000000, -1.000000000000000000 ) ) ;
#16308 = CIRCLE ( 'NONE', #7838, 20.00000000000000000 ) ;
#16309 = CARTESIAN_POINT ( 'NONE',  ( 3.160591952521659032, -3.281206521718069258, -0.8000000000000000444 ) ) ;
#16310 = LINE ( 'NONE', #2884, #4312 ) ;
#16311 = CARTESIAN_POINT ( 'NONE',  ( 57.36023556966787851, 55.99948385550239038, -0.02388180880522424582 ) ) ;
#16312 = CIRCLE ( 'NONE', #7213, 24.99999999999999289 ) ;
#16313 = DIRECTION ( 'NONE',  ( -0.000000000000000000, -0.000000000000000000, -1.000000000000000000 ) ) ;
#16314 = CARTESIAN_POINT ( 'NONE',  ( 42.39856655714566358, 54.89948385550240317, 2.493737253992119207 ) ) ;
#16315 = CARTESIAN_POINT ( 'NONE',  ( 56.66441430157294690, 50.90051614449766504, -2.141517661632166281 ) ) ;
#16316 = CARTESIAN_POINT ( 'NONE',  ( -0.1085714285714285687, -3.798448662927795372, -0.8000000000000000444 ) ) ;
#16317 = AXIS2_PLACEMENT_3D ( 'NONE', #10978, #5189, #3541 ) ;
#16318 = ORIENTED_EDGE ( 'NONE', *, *, #3904, .T. ) ;
#16319 = ORIENTED_EDGE ( 'NONE', *, *, #4477, .F. ) ;
#16320 = CARTESIAN_POINT ( 'NONE',  ( -154.9999999999999716, -14.99999999999999645, 6.499999999999999112 ) ) ;
#16321 = ORIENTED_EDGE ( 'NONE', *, *, #18752, .T. ) ;
#16322 = CARTESIAN_POINT ( 'NONE',  ( 0.000000000000000000, 0.000000000000000000, 0.000000000000000000 ) ) ;
#16323 = CIRCLE ( 'NONE', #6917, 20.00000000000000000 ) ;
#16324 = ORIENTED_EDGE ( 'NONE', *, *, #1614, .F. ) ;
#16325 = DIRECTION ( 'NONE',  ( 0.000000000000000000, 0.000000000000000000, -1.000000000000000000 ) ) ;
#16326 = EDGE_LOOP ( 'NONE', ( #9102, #9537, #16849, #4527, #15639, #11601, #14340 ) ) ;
#16327 = FACE_OUTER_BOUND ( 'NONE', #19141, .T. ) ;
#16328 = ORIENTED_EDGE ( 'NONE', *, *, #12881, .T. ) ;
#16329 = LINE ( 'NONE', #19391, #7409 ) ;
#16330 = FACE_OUTER_BOUND ( 'NONE', #14537, .T. ) ;
#16331 = CARTESIAN_POINT ( 'NONE',  ( 55.11794222512601493, 60.19948385550240744, 3.688883143319541702 ) ) ;
#16332 = FACE_BOUND ( 'NONE', #6842, .T. ) ;
#16333 = CARTESIAN_POINT ( 'NONE',  ( -155.0712099064782876, -18.99936609342274707, -15.00000000000000000 ) ) ;
#16334 = AXIS2_PLACEMENT_3D ( 'NONE', #13297, #16448, #15067 ) ;
#16335 = CIRCLE ( 'NONE', #6914, 5.899999999999999467 ) ;
#16336 = CARTESIAN_POINT ( 'NONE',  ( 58.41169779390614281, 51.00051614449765935, 0.02388180880515032231 ) ) ;
#16337 = CARTESIAN_POINT ( 'NONE',  ( 53.54508667620424234, 50.70051614449766220, -4.840751629271188961 ) ) ;
#16338 = DIRECTION ( 'NONE',  ( 0.000000000000000000, 0.000000000000000000, 1.000000000000000000 ) ) ;
#16339 = DIRECTION ( 'NONE',  ( 1.000000000000000000, 0.000000000000000000, 0.000000000000000000 ) ) ;
#16340 = VERTEX_POINT ( 'NONE', #18866 ) ;
#16341 = ORIENTED_EDGE ( 'NONE', *, *, #2816, .T. ) ;
#16342 = DIRECTION ( 'NONE',  ( 0.1305261922200521840, 0.9914448613738103822, -0.000000000000000000 ) ) ;
#16343 = ORIENTED_EDGE ( 'NONE', *, *, #1539, .T. ) ;
#16344 = EDGE_CURVE ( 'NONE', #153, #4928, #18175, .T. ) ;
#16345 = CARTESIAN_POINT ( 'NONE',  ( 43.33558569842703179, 63.09948385550240602, -2.141517661632099223 ) ) ;
#16346 = CARTESIAN_POINT ( 'NONE',  ( 5.599999999999999645, 2.020725942163688504, 3.500000000000000000 ) ) ;
#16347 = ORIENTED_EDGE ( 'NONE', *, *, #1731, .T. ) ;
#16348 = DIRECTION ( 'NONE',  ( 0.000000000000000000, 0.000000000000000000, 1.000000000000000000 ) ) ;
#16349 = EDGE_CURVE ( 'NONE', #14264, #15631, #3945, .T. ) ;
#16350 = PRODUCT ( 'reel holder bar', 'reel holder bar', '', ( #17766 ) ) ;
#16351 = CARTESIAN_POINT ( 'NONE',  ( 42.63976443033212149, 46.99948385550240459, 0.02388180880522514787 ) ) ;
#16352 = EDGE_CURVE ( 'NONE', #71, #9774, #8444, .T. ) ;
#16353 = CONICAL_SURFACE ( 'NONE', #6012, 2.059999999999998721, 0.9599310885968738161 ) ;
#16354 = EDGE_LOOP ( 'NONE', ( #5724, #14338, #3417, #1639 ) ) ;
#16355 = CARTESIAN_POINT ( 'NONE',  ( -14.14213562373094213, -14.99999999999998757, -50.00000000000000000 ) ) ;
#16356 = ORIENTED_EDGE ( 'NONE', *, *, #9976, .F. ) ;
#16357 = CARTESIAN_POINT ( 'NONE',  ( 2.449293598294706513E-15, -20.00000000000000000, -9.000000000000000000 ) ) ;
#16358 = ADVANCED_FACE ( 'NONE', ( #17092 ), #6973, .T. ) ;
#16359 = EDGE_CURVE ( 'NONE', #983, #15909, #3651, .T. ) ;
#16360 = CARTESIAN_POINT ( 'NONE',  ( 47.74827507625478518, 56.59948385550238470, 7.007379884777227730 ) ) ;
#16361 = CYLINDRICAL_SURFACE ( 'NONE', #12134, 2.500000000000000444 ) ;
#16362 = CARTESIAN_POINT ( 'NONE',  ( 57.36023556966787851, 53.00051614449765225, 0.02388180880515038476 ) ) ;
#16363 = CYLINDRICAL_SURFACE ( 'NONE', #18344, 1.000000000000000888 ) ;
#16364 = ADVANCED_FACE ( 'NONE', ( #5710, #4437 ), #10401, .F. ) ;
#16365 = CARTESIAN_POINT ( 'NONE',  ( 0.000000000000000000, 0.000000000000000000, -1.000000000000000000 ) ) ;
#16366 = CARTESIAN_POINT ( 'NONE',  ( 4.200000000000001954, 0.000000000000000000, 2.000000000000000888 ) ) ;
#16367 = ORIENTED_EDGE ( 'NONE', *, *, #18699, .F. ) ;
#16368 = PRODUCT_DEFINITION_SHAPE ( 'NONE', 'NONE',  #19427 ) ;
#16369 = EDGE_LOOP ( 'NONE', ( #12387, #8170, #17747, #8175 ) ) ;
#16370 = ORIENTED_EDGE ( 'NONE', *, *, #13584, .T. ) ;
#16371 = CARTESIAN_POINT ( 'NONE',  ( 0.1739375980333479343, -3.358985280702903253, -4.182066831946573693 ) ) ;
#16372 = EDGE_CURVE ( 'NONE', #7491, #439, #7464, .T. ) ;
#16373 = CARTESIAN_POINT ( 'NONE',  ( 47.42335538002188144, 64.59948385550241312, 8.007379884777233059 ) ) ;
#16374 = EDGE_CURVE ( 'NONE', #4248, #13076, #3140, .T. ) ;
#16375 = DIRECTION ( 'NONE',  ( 0.000000000000000000, -0.5000000000000011102, -0.8660254037844379305 ) ) ;
#16376 = VERTEX_POINT ( 'NONE', #8737 ) ;
#16377 = DIRECTION ( 'NONE',  ( -0.000000000000000000, -0.000000000000000000, -1.000000000000000000 ) ) ;
#16378 = VECTOR ( 'NONE', #7103, 1000.000000000000000 ) ;
#16379 = ORIENTED_EDGE ( 'NONE', *, *, #14825, .T. ) ;
#16380 = CARTESIAN_POINT ( 'NONE',  ( 52.25172492374528588, 57.40051614449765793, 7.007379884777204637 ) ) ;
#16381 = ORIENTED_EDGE ( 'NONE', *, *, #534, .F. ) ;
#16382 = CARTESIAN_POINT ( 'NONE',  ( 2.000000000000008882, 3.464101615137749945, 0.000000000000000000 ) ) ;
#16383 = UNCERTAINTY_MEASURE_WITH_UNIT (LENGTH_MEASURE( 1.000000000000000082E-05 ), #13001, 'distance_accuracy_value', 'NONE');
#16384 = CARTESIAN_POINT ( 'NONE',  ( 2.385244779468109755E-15, -20.00000000000000000, -9.999999999999994671 ) ) ;
#16385 = CARTESIAN_POINT ( 'NONE',  ( 51.97223112728249816, 50.60051614449765367, -5.992620115222793586 ) ) ;
#16386 = CARTESIAN_POINT ( 'NONE',  ( -154.9999999999999716, -14.99999999999999645, 6.499999999999999112 ) ) ;
#16387 = DIRECTION ( 'NONE',  ( -0.000000000000000000, -0.000000000000000000, -1.000000000000000000 ) ) ;
#16388 = CARTESIAN_POINT ( 'NONE',  ( 51.97223112728254790, 54.39948385550241028, 5.992620115222778487 ) ) ;
#16389 = CYLINDRICAL_SURFACE ( 'NONE', #17908, 2.000000000000000888 ) ;
#16390 = CARTESIAN_POINT ( 'NONE',  ( 42.63976443033212860, 54.99948385550241170, 0.02388180880522514787 ) ) ;
#16391 = CARTESIAN_POINT ( 'NONE',  ( 58.41169779390614281, 57.00051614449766646, 0.02388180880515032231 ) ) ;
#16392 = CARTESIAN_POINT ( 'NONE',  ( 18.00000000000000355, -20.00000000000000000, -12.00000000000000000 ) ) ;
#16393 = CARTESIAN_POINT ( 'NONE',  ( -4.207491450040567571, 2.029819825146470524, -3.671670828759566074 ) ) ;
#16394 = EDGE_LOOP ( 'NONE', ( #6977, #11500, #18882, #12717 ) ) ;
#16395 = DIRECTION ( 'NONE',  ( -0.000000000000000000, -0.000000000000000000, 1.000000000000000000 ) ) ;
#16396 = FILL_AREA_STYLE_COLOUR ( '', #9716 ) ;
#16397 = APPLICATION_PROTOCOL_DEFINITION ( 'draft international standard', 'automotive_design', 1998, #2888 ) ;
#16398 = PRODUCT_DEFINITION_FORMATION_WITH_SPECIFIED_SOURCE ( 'ANY', '', #17289, .NOT_KNOWN. ) ;
#16399 = VERTEX_POINT ( 'NONE', #10109 ) ;
#16400 = DIRECTION ( 'NONE',  ( 0.1045284632676635322, -0.9945218953682722907, 0.000000000000000000 ) ) ;
#16401 = CARTESIAN_POINT ( 'NONE',  ( -154.9999999999999716, -14.99999999999999645, -3.999999999999999112 ) ) ;
#16402 = CARTESIAN_POINT ( 'NONE',  ( 0.1217565302851118803, -3.710888496608922171, 0.5725525826504672677 ) ) ;
#16403 = CARTESIAN_POINT ( 'NONE',  ( 6.385552186430388133, 2.886751345948125991, 4.999999999999999112 ) ) ;
#16404 = DIRECTION ( 'NONE',  ( 1.000000000000000000, 0.000000000000000000, 0.000000000000000000 ) ) ;
#16405 = CARTESIAN_POINT ( 'NONE',  ( -162.9999999999999716, -14.99999999999999645, 15.00000000000000000 ) ) ;
#16406 = CARTESIAN_POINT ( 'NONE',  ( 47.74827507625478518, 60.59948385550239891, 7.007379884777227730 ) ) ;
#16407 = DIRECTION ( 'NONE',  ( 1.000000000000000000, 0.000000000000000000, 0.000000000000000000 ) ) ;
#16408 = CARTESIAN_POINT ( 'NONE',  ( 45.31609314410967926, 56.69948385550240744, 6.485486291978119766 ) ) ;
#16409 = FACE_OUTER_BOUND ( 'NONE', #15958, .T. ) ;
#16410 = CARTESIAN_POINT ( 'NONE',  ( 45.86712807150329496, 57.70051614449765509, 5.649768623646139964 ) ) ;
#16411 = EDGE_CURVE ( 'NONE', #7030, #8408, #19260, .T. ) ;
#16412 = CARTESIAN_POINT ( 'NONE',  ( -154.9999999999999716, -14.99999999999999645, -10.00000000000000000 ) ) ;
#16413 = VERTEX_POINT ( 'NONE', #10006 ) ;
#16414 = EDGE_CURVE ( 'NONE', #18086, #2369, #15963, .T. ) ;
#16415 = AXIS2_PLACEMENT_3D ( 'NONE', #8865, #10325, #6214 ) ;
#16416 = SHAPE_REPRESENTATION_RELATIONSHIP ( 'NONE' , 'NONE' ,  #8665, #18337 ) ;
#16417 = ORIENTED_EDGE ( 'NONE', *, *, #11297, .F. ) ;
#16418 = ORIENTED_EDGE ( 'NONE', *, *, #8064, .T. ) ;
#16419 = AXIS2_PLACEMENT_3D ( 'NONE', #12961, #9917, #2502 ) ;
#16420 = CARTESIAN_POINT ( 'NONE',  ( -62.49999999999997158, 32.50000000000001421, 15.00000000000000000 ) ) ;
#16421 = VERTEX_POINT ( 'NONE', #17874 ) ;
#16422 = CARTESIAN_POINT ( 'NONE',  ( -1.000000000000000222, -4.808326913195983821, 0.000000000000000000 ) ) ;
#16423 = ORIENTED_EDGE ( 'NONE', *, *, #11327, .T. ) ;
#16424 = CARTESIAN_POINT ( 'NONE',  ( 0.000000000000000000, 0.4273491293402468805, -0.8000000000000000444 ) ) ;
#16425 = ORIENTED_EDGE ( 'NONE', *, *, #7900, .T. ) ;
#16426 = DIRECTION ( 'NONE',  ( 0.03086419753086420623, 0.9995235871707959241, -0.000000000000000000 ) ) ;
#16427 = DIRECTION ( 'NONE',  ( 0.000000000000000000, 0.000000000000000000, 1.000000000000000000 ) ) ;
#16428 = CARTESIAN_POINT ( 'NONE',  ( 50.02271294988511841, 54.49948385550240459, 6.000000000000000888 ) ) ;
#16429 = DIRECTION ( 'NONE',  ( -1.000000000000000000, -4.082155997157843695E-16, 0.000000000000000000 ) ) ;
#16430 = FILL_AREA_STYLE_COLOUR ( '', #7044 ) ;
#16431 =( REPRESENTATION_RELATIONSHIP ('NONE','NONE', #16703, #13919 ) REPRESENTATION_RELATIONSHIP_WITH_TRANSFORMATION ( #12543 )SHAPE_REPRESENTATION_RELATIONSHIP( ) );
#16432 = CARTESIAN_POINT ( 'NONE',  ( 58.41169779390614281, 53.00051614449765935, 0.02388180880515032231 ) ) ;
#16433 = VECTOR ( 'NONE', #5194, 1000.000000000000000 ) ;
#16434 = CARTESIAN_POINT ( 'NONE',  ( 53.50833635130544508, 49.30051614449766362, 4.867452303228181343 ) ) ;
#16435 = DIRECTION ( 'NONE',  ( 4.082155997157843695E-16, -1.000000000000000000, 0.000000000000000000 ) ) ;
#16436 = PLANE ( 'NONE',  #7196 ) ;
#16437 = ORIENTED_EDGE ( 'NONE', *, *, #10875, .F. ) ;
#16438 = ORIENTED_EDGE ( 'NONE', *, *, #8556, .F. ) ;
#16439 = CARTESIAN_POINT ( 'NONE',  ( -3.349226789952655547, -2.685125164760744809, -0.2236248678334863682 ) ) ;
#16440 = VERTEX_POINT ( 'NONE', #14515 ) ;
#16441 = CARTESIAN_POINT ( 'NONE',  ( 54.13287192849676188, 62.29948385550240886, 5.649768623646098220 ) ) ;
#16442 = PLANE ( 'NONE',  #16570 ) ;
#16443 = ORIENTED_EDGE ( 'NONE', *, *, #5168, .T. ) ;
#16444 = CIRCLE ( 'NONE', #17382, 0.9999999999999997780 ) ;
#16445 = CARTESIAN_POINT ( 'NONE',  ( -0.1481481481481481122, -4.797713218419819903, -1.000000000000000000 ) ) ;
#16446 = DIRECTION ( 'NONE',  ( -0.000000000000000000, -0.000000000000000000, -1.000000000000000000 ) ) ;
#16447 = ORIENTED_EDGE ( 'NONE', *, *, #11542, .T. ) ;
#16448 = DIRECTION ( 'NONE',  ( -0.000000000000000000, -0.000000000000000000, 1.000000000000000000 ) ) ;
#16449 = VERTEX_POINT ( 'NONE', #4143 ) ;
#16450 = CARTESIAN_POINT ( 'NONE',  ( 50.02271294988505446, 62.50051614449767357, -8.000000000000001776 ) ) ;
#16451 = CARTESIAN_POINT ( 'NONE',  ( -6.080745460913608902, 0.5192545390863924082, -1.000000000000000000 ) ) ;
#16452 = AXIS2_PLACEMENT_3D ( 'NONE', #11761, #19165, #1196 ) ;
#16453 = CARTESIAN_POINT ( 'NONE',  ( 45.90387839640214196, 60.69948385550240033, 5.676469297603166098 ) ) ;
#16454 = LINE ( 'NONE', #3309, #13225 ) ;
#16455 = PRESENTATION_STYLE_ASSIGNMENT (( #10743 ) ) ;
#16456 = CARTESIAN_POINT ( 'NONE',  ( 55.94051828345053679, 53.20051614449766220, 4.345558710429044069 ) ) ;
#16457 = CARTESIAN_POINT ( 'NONE',  ( -158.9999999999999716, -14.99999999999999645, -10.00000000000000178 ) ) ;
#16458 = EDGE_CURVE ( 'NONE', #6603, #8359, #11253, .T. ) ;
#16459 = DIRECTION ( 'NONE',  ( 0.000000000000000000, 0.000000000000000000, 1.000000000000000000 ) ) ;
#16460 = VECTOR ( 'NONE', #18229, 1000.000000000000000 ) ;
#16461 = CARTESIAN_POINT ( 'NONE',  ( 2.449293598294706513E-15, -20.00000000000000000, -20.00000000000000000 ) ) ;
#16462 = ORIENTED_EDGE ( 'NONE', *, *, #4020, .F. ) ;
#16463 = ORIENTED_EDGE ( 'NONE', *, *, #4827, .T. ) ;
#16464 = ORIENTED_EDGE ( 'NONE', *, *, #13988, .T. ) ;
#16465 = CARTESIAN_POINT ( 'NONE',  ( -62.49999999999997158, 45.00000000000001421, 0.000000000000000000 ) ) ;
#16466 = CIRCLE ( 'NONE', #5175, 4.000000000000000000 ) ;
#16467 = CARTESIAN_POINT ( 'NONE',  ( 52.62207051974839089, 64.39948385550239607, 7.992620115222770494 ) ) ;
#16468 =( NAMED_UNIT ( * ) SI_UNIT ( $, .STERADIAN. ) SOLID_ANGLE_UNIT ( ) );
#16469 = VERTEX_POINT ( 'NONE', #13445 ) ;
#16470 = CARTESIAN_POINT ( 'NONE',  ( -154.9999999999999716, -14.99999999999999645, 17.00000000000000000 ) ) ;
#16471 = EDGE_CURVE ( 'NONE', #15972, #13265, #6257, .T. ) ;
#16472 = ORIENTED_EDGE ( 'NONE', *, *, #14578, .F. ) ;
#16473 = CARTESIAN_POINT ( 'NONE',  ( 44.03140696652198471, 61.80051614449766362, 4.306917132069485454 ) ) ;
#16474 = EDGE_LOOP ( 'NONE', ( #16775, #6852 ) ) ;
#16475 = PLANE ( 'NONE',  #5670 ) ;
#16476 = LINE ( 'NONE', #2395, #14933 ) ;
#16477 = CARTESIAN_POINT ( 'NONE',  ( 56.30877334542961421, 53.00051614449765935, 0.02388180880515774693 ) ) ;
#16478 = DIRECTION ( 'NONE',  ( -1.000000000000000000, 0.000000000000000000, 0.000000000000000000 ) ) ;
#16479 = VECTOR ( 'NONE', #10948, 1000.000000000000000 ) ;
#16480 = EDGE_CURVE ( 'NONE', #14983, #8685, #9061, .T. ) ;
#16481 = DIRECTION ( 'NONE',  ( -0.000000000000000000, 0.000000000000000000, -1.000000000000000000 ) ) ;
#16482 = EDGE_CURVE ( 'NONE', #10947, #4767, #13248, .T. ) ;
#16483 = CARTESIAN_POINT ( 'NONE',  ( 44.28664221472220675, 55.09948385550241312, -1.832500667257165317 ) ) ;
#16484 = CARTESIAN_POINT ( 'NONE',  ( 3.436319922986518449, -2.634841920959471562, -3.531542292954761741 ) ) ;
#16485 = CARTESIAN_POINT ( 'NONE',  ( 43.20883090819742023, 52.20051614449766220, -4.963592699178938972 ) ) ;
#16486 = CARTESIAN_POINT ( 'NONE',  ( 6.357976367241810145, -3.426708043488799760, 4.282301071214263288 ) ) ;
#16487 = FACE_OUTER_BOUND ( 'NONE', #14730, .T. ) ;
#16488 = PRESENTATION_LAYER_ASSIGNMENT (  '', '', ( #6750 ) ) ;
#16489 = DIRECTION ( 'NONE',  ( -1.000000000000000000, 0.000000000000000000, 0.000000000000000000 ) ) ;
#16490 = CARTESIAN_POINT ( 'NONE',  ( 0.000000000000000000, 0.000000000000000000, 0.000000000000000000 ) ) ;
#16491 = EDGE_CURVE ( 'NONE', #11186, #1055, #6873, .T. ) ;
#16492 = SHAPE_DEFINITION_REPRESENTATION ( #14124, #17450 ) ;
#16493 = ADVANCED_FACE ( 'NONE', ( #11763 ), #5501, .F. ) ;
#16494 = ORIENTED_EDGE ( 'NONE', *, *, #17259, .F. ) ;
#16495 = PLANE ( 'NONE',  #9862 ) ;
#16496 = ADVANCED_FACE ( 'NONE', ( #19362 ), #2777, .T. ) ;
#16497 = CARTESIAN_POINT ( 'NONE',  ( 19.30627432446651781, -25.22185519795838715, -9.000000000000000000 ) ) ;
#16498 = CARTESIAN_POINT ( 'NONE',  ( 52.29715082351547295, 64.39948385550239607, 6.992620115222774047 ) ) ;
#16499 = CARTESIAN_POINT ( 'NONE',  ( 0.9999999999999997780, -6.008326913195983998, 0.000000000000000000 ) ) ;
#16500 = FACE_OUTER_BOUND ( 'NONE', #18255, .T. ) ;
#16501 = CARTESIAN_POINT ( 'NONE',  ( -155.0777214229742071, -18.79920509849242549, 15.79999999999999893 ) ) ;
#16502 = CARTESIAN_POINT ( 'NONE',  ( 45.90387839640214196, 58.69948385550240033, 5.676469297603166098 ) ) ;
#16503 = LINE ( 'NONE', #13736, #5132 ) ;
#16504 = CIRCLE ( 'NONE', #16192, 1.000000000000000222 ) ;
#16505 = CARTESIAN_POINT ( 'NONE',  ( 56.79116909180255135, 51.79948385550240175, -4.963592699179005585 ) ) ;
#16506 = CARTESIAN_POINT ( 'NONE',  ( 3.961551342853212532, -2.319461885623237851, -2.982574167881048677 ) ) ;
#16507 = CARTESIAN_POINT ( 'NONE',  ( 52.25172492374527877, 53.40051614449765793, 7.007379884777203749 ) ) ;
#16508 = LINE ( 'NONE', #10208, #6282 ) ;
#16509 = ORIENTED_EDGE ( 'NONE', *, *, #17722, .F. ) ;
#16510 = VECTOR ( 'NONE', #11868, 1000.000000000000000 ) ;
#16511 = ORIENTED_EDGE ( 'NONE', *, *, #4590, .T. ) ;
#16512 = AXIS2_PLACEMENT_3D ( 'NONE', #11604, #10131, #8663 ) ;
#16513 = LINE ( 'NONE', #18088, #10 ) ;
#16514 = VECTOR ( 'NONE', #6172, 1000.000000000000000 ) ;
#16515 = ORIENTED_EDGE ( 'NONE', *, *, #16471, .F. ) ;
#16516 = DIRECTION ( 'NONE',  ( -0.000000000000000000, -0.000000000000000000, 1.000000000000000000 ) ) ;
#16517 = EDGE_CURVE ( 'NONE', #18690, #11822, #10949, .T. ) ;
#16518 = CARTESIAN_POINT ( 'NONE',  ( 52.25172492374522903, 63.59948385550237759, -7.007379884777225953 ) ) ;
#16519 = CARTESIAN_POINT ( 'NONE',  ( -150.9999999999999716, -14.99999999999999645, -10.00000000000000178 ) ) ;
#16520 = VERTEX_POINT ( 'NONE', #5603 ) ;
#16521 = CARTESIAN_POINT ( 'NONE',  ( 2.500000000000000444, 0.000000000000000000, -25.03750572909317285 ) ) ;
#16522 = CARTESIAN_POINT ( 'NONE',  ( 2.000000000000000000, -1.773042676681341856, 2.276824562219559311E-15 ) ) ;
#16523 = EDGE_CURVE ( 'NONE', #3708, #7017, #11574, .T. ) ;
#16524 = CARTESIAN_POINT ( 'NONE',  ( 53.54508667620428497, 54.29948385550241596, 4.840751629271157874 ) ) ;
#16525 = LINE ( 'NONE', #13757, #15733 ) ;
#16526 = DIRECTION ( 'NONE',  ( -1.000000000000000000, 0.000000000000000000, -0.000000000000000000 ) ) ;
#16527 = AXIS2_PLACEMENT_3D ( 'NONE', #5007, #15495, #18658 ) ;
#16528 = CARTESIAN_POINT ( 'NONE',  ( 43.18075615816994173, 53.80051614449766362, 4.924951120819380357 ) ) ;
#16529 = CARTESIAN_POINT ( 'NONE',  ( 49.97728705011494554, 53.50051614449767357, 6.000000000000000888 ) ) ;
#16530 = AXIS2_PLACEMENT_3D ( 'NONE', #9812, #1013, #10111 ) ;
#16531 = DIRECTION ( 'NONE',  ( -0.1045284632676425907, -0.9945218953682745111, 0.000000000000000000 ) ) ;
#16532 = DIRECTION ( 'NONE',  ( 0.000000000000000000, 0.000000000000000000, -1.000000000000000000 ) ) ;
#16533 = VERTEX_POINT ( 'NONE', #4330 ) ;
#16534 = ORIENTED_EDGE ( 'NONE', *, *, #6869, .T. ) ;
#16535 = DIRECTION ( 'NONE',  ( -1.000000000000000000, 0.000000000000000000, 0.000000000000000000 ) ) ;
#16536 = ORIENTED_EDGE ( 'NONE', *, *, #4224, .F. ) ;
#16537 = CARTESIAN_POINT ( 'NONE',  ( 47.74827507625478518, 64.59948385550239891, 7.007379884777227730 ) ) ;
#16538 = FACE_OUTER_BOUND ( 'NONE', #3208, .T. ) ;
#16539 = CIRCLE ( 'NONE', #8992, 14.00000000000000000 ) ;
#16540 = ORIENTED_EDGE ( 'NONE', *, *, #4256, .F. ) ;
#16541 = CARTESIAN_POINT ( 'NONE',  ( 2.886521338340684917, 0.000000000000000000, 0.000000000000000000 ) ) ;
#16542 = CARTESIAN_POINT ( 'NONE',  ( -74.99999999999997158, 1.000000000000000000, 6.000000000000000000 ) ) ;
#16543 = ADVANCED_FACE ( 'NONE', ( #7272 ), #17588, .T. ) ;
#16544 = AXIS2_PLACEMENT_3D ( 'NONE', #17378, #7065, #2482 ) ;
#16545 = ORIENTED_EDGE ( 'NONE', *, *, #9721, .T. ) ;
#16546 = DIRECTION ( 'NONE',  ( 0.000000000000000000, 1.000000000000000000, -1.345283343056720273E-15 ) ) ;
#16547 = EDGE_LOOP ( 'NONE', ( #15848, #14683, #4771, #47 ) ) ;
#16548 = CARTESIAN_POINT ( 'NONE',  ( 47.37792948025170858, 63.60051614449764656, 7.992620115222797139 ) ) ;
#16549 = CARTESIAN_POINT ( 'NONE',  ( 50.38494826773854385, 45.00000000000002842, -6.500000000000005329 ) ) ;
#16550 = CARTESIAN_POINT ( 'NONE',  ( 52.25172492374522903, 55.59948385550241312, -7.007379884777225953 ) ) ;
#16551 = DIRECTION ( 'NONE',  ( 0.03933706530295848214, -0.9992259981072103558, 7.446367396525006349E-17 ) ) ;
#16552 = DIRECTION ( 'NONE',  ( -0.000000000000000000, -0.000000000000000000, -1.000000000000000000 ) ) ;
#16553 = CARTESIAN_POINT ( 'NONE',  ( 52.25172492374527877, 51.40051614449767214, 7.007379884777203749 ) ) ;
#16554 = DIRECTION ( 'NONE',  ( 1.000000000000000000, 0.000000000000000000, 0.000000000000000000 ) ) ;
#16555 = LINE ( 'NONE', #17939, #14260 ) ;
#16556 = DIRECTION ( 'NONE',  ( -1.000000000000000000, -0.000000000000000000, -0.000000000000000000 ) ) ;
#16557 = EDGE_LOOP ( 'NONE', ( #6006, #9764, #8286, #19380 ) ) ;
#16558 = MECHANICAL_DESIGN_GEOMETRIC_PRESENTATION_REPRESENTATION (  '', ( #574 ), #8076 ) ;
#16559 = AXIS2_PLACEMENT_3D ( 'NONE', #13902, #398, #3438 ) ;
#16560 = VERTEX_POINT ( 'NONE', #8638 ) ;
#16561 = ORIENTED_EDGE ( 'NONE', *, *, #301, .T. ) ;
#16562 = FACE_OUTER_BOUND ( 'NONE', #879, .T. ) ;
#16563 = CARTESIAN_POINT ( 'NONE',  ( 57.60143344285433642, 63.89948385550240317, -2.493737253992118319 ) ) ;
#16564 = CARTESIAN_POINT ( 'NONE',  ( -59.84999999999998721, 32.50000000000001421, 9.999999999999998224 ) ) ;
#16565 = VERTEX_POINT ( 'NONE', #3256 ) ;
#16566 = CARTESIAN_POINT ( 'NONE',  ( 6.533910050139697390, 5.901028503456123175, 1.520834953648585461E-14 ) ) ;
#16567 = ORIENTED_EDGE ( 'NONE', *, *, #14753, .T. ) ;
#16568 = CARTESIAN_POINT ( 'NONE',  ( 45.90387839640208512, 58.30051614449766362, -5.676469297603124353 ) ) ;
#16569 = VERTEX_POINT ( 'NONE', #16497 ) ;
#16570 = AXIS2_PLACEMENT_3D ( 'NONE', #16346, #14759, #1642 ) ;
#16571 = VECTOR ( 'NONE', #17817, 1000.000000000000000 ) ;
#16572 = PLANE ( 'NONE',  #15048 ) ;
#16573 = UNCERTAINTY_MEASURE_WITH_UNIT (LENGTH_MEASURE( 1.000000000000000082E-05 ), #7576, 'distance_accuracy_value', 'NONE');
#16574 = DIRECTION ( 'NONE',  ( -1.000000000000000000, 0.000000000000000000, 0.000000000000000000 ) ) ;
#16575 = CARTESIAN_POINT ( 'NONE',  ( 44.91013252490150620, 54.20051614449766220, -3.727524721679154940 ) ) ;
#16576 = DIRECTION ( 'NONE',  ( -0.000000000000000000, -0.000000000000000000, -1.000000000000000000 ) ) ;
#16577 = DIRECTION ( 'NONE',  ( 0.6691306063588571273, 0.7431448254773952433, 0.000000000000000000 ) ) ;
#16578 = CARTESIAN_POINT ( 'NONE',  ( 55.71335778527780747, 58.09948385550241312, 1.832500667257165983 ) ) ;
#16579 = LINE ( 'NONE', #201, #10662 ) ;
#16580 = CARTESIAN_POINT ( 'NONE',  ( 49.97728705011495265, 53.50051614449767357, 8.000000000000001776 ) ) ;
#16581 = CARTESIAN_POINT ( 'NONE',  ( 1.267864665261691752E-11, -20.00000000000000000, 9.999999999999998224 ) ) ;
#16582 = DIRECTION ( 'NONE',  ( -0.000000000000000000, -0.000000000000000000, 1.000000000000000000 ) ) ;
#16583 = ORIENTED_EDGE ( 'NONE', *, *, #2247, .T. ) ;
#16584 = DIRECTION ( 'NONE',  ( 0.000000000000000000, 0.000000000000000000, -1.000000000000000000 ) ) ;
#16585 = FILL_AREA_STYLE ('',( #10868 ) ) ;
#16586 = CIRCLE ( 'NONE', #11869, 0.7500000000000000000 ) ;
#16587 = VECTOR ( 'NONE', #11813, 1000.000000000000000 ) ;
#16588 = APPLICATION_PROTOCOL_DEFINITION ( 'draft international standard', 'automotive_design', 1998, #18288 ) ;
#16589 = ORIENTED_EDGE ( 'NONE', *, *, #5599, .T. ) ;
#16590 = LINE ( 'NONE', #10399, #482 ) ;
#16591 = EDGE_CURVE ( 'NONE', #18521, #10636, #20, .T. ) ;
#16592 = DIRECTION ( 'NONE',  ( -0.000000000000000000, -0.000000000000000000, 1.000000000000000000 ) ) ;
#16593 = EDGE_CURVE ( 'NONE', #983, #3316, #9216, .T. ) ;
#16594 = CARTESIAN_POINT ( 'NONE',  ( 56.66441430157296821, 62.09948385550239891, 2.141517661632100111 ) ) ;
#16595 = LINE ( 'NONE', #13447, #2437 ) ;
#16596 = AXIS2_PLACEMENT_3D ( 'NONE', #3554, #18577, #12761 ) ;
#16597 = CARTESIAN_POINT ( 'NONE',  ( 6.196878017913834746, 1.924500897298752955, 5.000000000000000000 ) ) ;
#16598 = EDGE_CURVE ( 'NONE', #9092, #13632, #4818, .T. ) ;
#16599 = EDGE_CURVE ( 'NONE', #2802, #17741, #4388, .T. ) ;
#16600 = DIRECTION ( 'NONE',  ( 1.000000000000000000, 0.000000000000000000, 0.000000000000000000 ) ) ;
#16601 = CARTESIAN_POINT ( 'NONE',  ( 43.34962307344081012, 60.89948385550241028, 2.184720259617164650 ) ) ;
#16602 = DIRECTION ( 'NONE',  ( -1.000000000000000000, -0.000000000000000000, -0.000000000000000000 ) ) ;
#16603 = CARTESIAN_POINT ( 'NONE',  ( 56.79116909180255135, 53.79948385550241596, -4.963592699179005585 ) ) ;
#16604 = CARTESIAN_POINT ( 'NONE',  ( 4.158921614371310582, -4.076055977742308656, 0.05993604794450350243 ) ) ;
#16605 = CARTESIAN_POINT ( 'NONE',  ( 45.90387839640208512, 56.30051614449765651, -5.676469297603124353 ) ) ;
#16606 = EDGE_CURVE ( 'NONE', #11260, #9229, #3349, .T. ) ;
#16607 = AXIS2_PLACEMENT_3D ( 'NONE', #16581, #9209, #14069 ) ;
#16608 = PLANE ( 'NONE',  #18517 ) ;
#16609 =( NAMED_UNIT ( * ) SI_UNIT ( $, .STERADIAN. ) SOLID_ANGLE_UNIT ( ) );
#16610 = VERTEX_POINT ( 'NONE', #15397 ) ;
#16611 = VECTOR ( 'NONE', #11158, 1000.000000000000000 ) ;
#16612 = EDGE_CURVE ( 'NONE', #6443, #6347, #3446, .T. ) ;
#16613 = EDGE_CURVE ( 'NONE', #17604, #6538, #2532, .T. ) ;
#16614 = CARTESIAN_POINT ( 'NONE',  ( 2.290893957444128645E-15, 4.647089433458768681, -3.572167766733382877 ) ) ;
#16615 = VECTOR ( 'NONE', #12751, 1000.000000000000000 ) ;
#16616 = AXIS2_PLACEMENT_3D ( 'NONE', #17026, #5139, #17316 ) ;
#16617 = ORIENTED_EDGE ( 'NONE', *, *, #15006, .F. ) ;
#16618 = DIRECTION ( 'NONE',  ( -1.000000000000000000, 0.000000000000000000, 0.000000000000000000 ) ) ;
#16619 = CARTESIAN_POINT ( 'NONE',  ( 45.86712807150323812, 65.29948385550241596, -5.649768623646098220 ) ) ;
#16620 = CIRCLE ( 'NONE', #8143, 3.799999999999999378 ) ;
#16621 = DIRECTION ( 'NONE',  ( -0.000000000000000000, -0.000000000000000000, -1.000000000000000000 ) ) ;
#16622 = ORIENTED_EDGE ( 'NONE', *, *, #13945, .F. ) ;
#16623 = DIRECTION ( 'NONE',  ( 0.000000000000000000, -0.000000000000000000, 1.000000000000000000 ) ) ;
#16624 = FACE_OUTER_BOUND ( 'NONE', #16032, .T. ) ;
#16625 = CARTESIAN_POINT ( 'NONE',  ( 48.07319477248768180, 58.59948385550239891, 6.007379884777225953 ) ) ;
#16626 = DIRECTION ( 'NONE',  ( 4.082155997157843695E-16, -1.000000000000000000, 0.000000000000000000 ) ) ;
#16627 = DIRECTION ( 'NONE',  ( -0.000000000000000000, -0.000000000000000000, -1.000000000000000000 ) ) ;
#16628 = CARTESIAN_POINT ( 'NONE',  ( 57.60143344285435774, 55.10051614449765367, 2.493737253992045044 ) ) ;
#16629 = VECTOR ( 'NONE', #16674, 1000.000000000000000 ) ;
#16630 = CARTESIAN_POINT ( 'NONE',  ( 48.07319477248762496, 56.40051614449765793, -6.007379884777208190 ) ) ;
#16632 = AXIS2_PLACEMENT_3D ( 'NONE', #5567, #6943, #9783 ) ;
#16631 = CARTESIAN_POINT ( 'NONE',  ( 3.129923130707922496, -23.63917314727666152, -9.999999999999994671 ) ) ;
#16633 = AXIS2_PLACEMENT_3D ( 'NONE', #5523, #15931, #12889 ) ;
#16634 = FACE_BOUND ( 'NONE', #12729, .T. ) ;
#16635 = ORIENTED_EDGE ( 'NONE', *, *, #8476, .T. ) ;
#16636 = AXIS2_PLACEMENT_3D ( 'NONE', #12177, #16704, #6383 ) ;
#16637 = ORIENTED_EDGE ( 'NONE', *, *, #10774, .F. ) ;
#16638 = DIRECTION ( 'NONE',  ( -0.000000000000000000, -0.000000000000000000, 1.000000000000000000 ) ) ;
#16639 = ORIENTED_EDGE ( 'NONE', *, *, #15311, .T. ) ;
#16640 = CARTESIAN_POINT ( 'NONE',  ( 56.66441430157296821, 64.09948385550239891, 2.141517661632100111 ) ) ;
#16641 = DIRECTION ( 'NONE',  ( 0.000000000000000000, 0.000000000000000000, -1.000000000000000000 ) ) ;
#16642 = ORIENTED_EDGE ( 'NONE', *, *, #9264, .F. ) ;
#16643 = CARTESIAN_POINT ( 'NONE',  ( 0.000000000000000000, 0.000000000000000000, 8.999999999999998224 ) ) ;
#16644 = AXIS2_PLACEMENT_3D ( 'NONE', #13564, #16803, #4652 ) ;
#16645 = CARTESIAN_POINT ( 'NONE',  ( 0.4472135954999577612, 0.000000000000000000, 0.000000000000000000 ) ) ;
#16646 = ORIENTED_EDGE ( 'NONE', *, *, #14789, .T. ) ;
#16647 = LINE ( 'NONE', #16355, #7866 ) ;
#16648 = VECTOR ( 'NONE', #12016, 1000.000000000000000 ) ;
#16649 = ORIENTED_EDGE ( 'NONE', *, *, #9172, .T. ) ;
#16650 = CARTESIAN_POINT ( 'NONE',  ( 56.81924384183006538, 62.80051614449766362, -4.924951120819380357 ) ) ;
#16651 = AXIS2_PLACEMENT_3D ( 'NONE', #13483, #5838, #11808 ) ;
#16652 = DIRECTION ( 'NONE',  ( 0.000000000000000000, 0.000000000000000000, 1.000000000000000000 ) ) ;
#16653 = CARTESIAN_POINT ( 'NONE',  ( 55.96859303347804371, 58.19948385550241454, 4.306917132069425946 ) ) ;
#16654 = CARTESIAN_POINT ( 'NONE',  ( -62.49999999999997158, 45.00000000000001421, 9.999999999999998224 ) ) ;
#16655 = SURFACE_STYLE_FILL_AREA ( #12313 ) ;
#16656 = CARTESIAN_POINT ( 'NONE',  ( 45.90387839640208512, 54.30051614449765651, -5.676469297603124353 ) ) ;
#16657 = CARTESIAN_POINT ( 'NONE',  ( 0.000000000000000000, 0.000000000000000000, 0.000000000000000000 ) ) ;
#16658 = DIRECTION ( 'NONE',  ( 0.000000000000000000, -9.783878858594328898E-16, -1.000000000000000000 ) ) ;
#16659 = VERTEX_POINT ( 'NONE', #10689 ) ;
#16660 = EDGE_CURVE ( 'NONE', #9835, #16565, #7562, .T. ) ;
#16661 = VECTOR ( 'NONE', #8477, 1000.000000000000000 ) ;
#16662 = EDGE_LOOP ( 'NONE', ( #4376, #12593, #4019, #10445 ) ) ;
#16663 = ORIENTED_EDGE ( 'NONE', *, *, #17138, .T. ) ;
#16664 = DIRECTION ( 'NONE',  ( 0.000000000000000000, 0.000000000000000000, 1.000000000000000000 ) ) ;
#16665 = FILL_AREA_STYLE ('',( #10658 ) ) ;
#16666 = EDGE_CURVE ( 'NONE', #12888, #14141, #1579, .T. ) ;
#16667 = CARTESIAN_POINT ( 'NONE',  ( 54.13287192849676188, 48.29948385550240175, 5.649768623646098220 ) ) ;
#16668 = CIRCLE ( 'NONE', #10064, 4.000000000000031086 ) ;
#16669 = ORIENTED_EDGE ( 'NONE', *, *, #16139, .F. ) ;
#16670 = CARTESIAN_POINT ( 'NONE',  ( 2.449293598294706513E-15, -20.00000000000000000, 9.000000000000000000 ) ) ;
#16671 = ORIENTED_EDGE ( 'NONE', *, *, #7284, .T. ) ;
#16672 = CARTESIAN_POINT ( 'NONE',  ( 54.09612160359792199, 57.30051614449765651, 5.676469297603124353 ) ) ;
#16673 = EDGE_LOOP ( 'NONE', ( #19325, #12139, #1036, #191 ) ) ;
#16674 = DIRECTION ( 'NONE',  ( 0.000000000000000000, -1.000000000000000000, 0.000000000000000000 ) ) ;
#16675 = DIRECTION ( 'NONE',  ( 0.1305261922200524338, -0.9914448613738102711, 0.000000000000000000 ) ) ;
#16676 = CARTESIAN_POINT ( 'NONE',  ( 46.45491332379576477, 57.70051614449766930, 4.840751629271188961 ) ) ;
#16677 = DIRECTION ( 'NONE',  ( -2.191393683118470056E-17, -7.538405132783724027E-17, -1.000000000000000000 ) ) ;
#16678 = CARTESIAN_POINT ( 'NONE',  ( 4.872650870659752442, 0.4273491293402468805, -0.8000000000000000444 ) ) ;
#16679 = AXIS2_PLACEMENT_3D ( 'NONE', #1500, #12173, #13353 ) ;
#16680 = CARTESIAN_POINT ( 'NONE',  ( 46.45491332379572924, 59.29948385550240886, -4.840751629271157874 ) ) ;
#16681 = DIRECTION ( 'NONE',  ( -1.000000000000000000, 0.000000000000000000, 0.000000000000000000 ) ) ;
#16682 = CARTESIAN_POINT ( 'NONE',  ( 52.57664461997821093, 55.40051614449767214, 8.007379884777206414 ) ) ;
#16683 = CARTESIAN_POINT ( 'NONE',  ( -14.99999999999999822, -19.99999999999999645, -50.00000000000000000 ) ) ;
#16684 = EDGE_LOOP ( 'NONE', ( #12005, #15059, #15734, #11548 ) ) ;
#16685 = FACE_OUTER_BOUND ( 'NONE', #2944, .T. ) ;
#16686 = CARTESIAN_POINT ( 'NONE',  ( 2.449293598294706513E-15, -20.00000000000000000, -9.000000000000000000 ) ) ;
#16687 = SHAPE_DEFINITION_REPRESENTATION ( #19198, #19357 ) ;
#16688 = CIRCLE ( 'NONE', #18890, 5.000000000000000888 ) ;
#16689 = ORIENTED_EDGE ( 'NONE', *, *, #4892, .F. ) ;
#16690 = CARTESIAN_POINT ( 'NONE',  ( 1.000000000000000000, -14.00000000000000000, -9.000000000000001776 ) ) ;
#16691 = DIRECTION ( 'NONE',  ( 1.000000000000000000, 0.000000000000000000, 0.000000000000000000 ) ) ;
#16692 = APPLICATION_CONTEXT ( 'automotive_design' ) ;
#16693 = CARTESIAN_POINT ( 'NONE',  ( 47.74827507625477807, 64.59948385550239891, 7.007379884777229506 ) ) ;
#16694 = CARTESIAN_POINT ( 'NONE',  ( 13.61000000000001009, 2.449293598294708386E-16, -2.000000000000001332 ) ) ;
#16695 = CARTESIAN_POINT ( 'NONE',  ( -9.999999999999996447, 0.000000000000000000, 9.999999999999998224 ) ) ;
#16696 = PLANE ( 'NONE',  #17466 ) ;
#16697 = CARTESIAN_POINT ( 'NONE',  ( 45.86712807150323812, 61.29948385550240886, -5.649768623646098220 ) ) ;
#16698 = DIRECTION ( 'NONE',  ( 0.000000000000000000, -1.000000000000000000, 9.783878858594328898E-16 ) ) ;
#16699 = CARTESIAN_POINT ( 'NONE',  ( 52.57664461997811856, 57.59948385550240602, -8.007379884777229506 ) ) ;
#16700 = ADVANCED_FACE ( 'NONE', ( #3165 ), #16883, .F. ) ;
#16701 = CARTESIAN_POINT ( 'NONE',  ( 45.86712807150329496, 55.70051614449766220, 5.649768623646139964 ) ) ;
#16702 = CARTESIAN_POINT ( 'NONE',  ( 2.449293598294706513E-15, -20.00000000000000000, 9.000000000000000000 ) ) ;
#16703 = SHAPE_REPRESENTATION ( 'MAS-177', ( #9470, #19096, #17839, #918, #11865, #3433, #4682, #297, #6236, #5289, #16266, #18470, #7796, #18779, #9986, #15012, #6549, #720, #11672, #18274, #3241, #3857, #13244, #6665, #12924 ), #6047 ) ;
#16704 = DIRECTION ( 'NONE',  ( -0.000000000000000000, -0.000000000000000000, 1.000000000000000000 ) ) ;
#16705 = ORIENTED_EDGE ( 'NONE', *, *, #2404, .F. ) ;
#16706 = CARTESIAN_POINT ( 'NONE',  ( 0.3126073911695746443, -2.020725942163797750, -3.499999999999999556 ) ) ;
#16707 = CARTESIAN_POINT ( 'NONE',  ( 47.70284917648459810, 49.60051614449765367, 6.992620115222797139 ) ) ;
#16708 = EDGE_CURVE ( 'NONE', #11235, #11423, #4081, .T. ) ;
#16709 = CARTESIAN_POINT ( 'NONE',  ( 56.66441430157296821, 64.09948385550239891, 2.141517661632100111 ) ) ;
#16710 = EDGE_CURVE ( 'NONE', #6066, #6353, #6370, .T. ) ;
#16711 = CARTESIAN_POINT ( 'NONE',  ( 30.00000000000000000, -40.00000000000000000, -5.999999999999998224 ) ) ;
#16712 = ORIENTED_EDGE ( 'NONE', *, *, #2404, .T. ) ;
#16713 = CARTESIAN_POINT ( 'NONE',  ( 9.037824375505316254, -2.158539001597377105, 0.000000000000000000 ) ) ;
#16714 = DIRECTION ( 'NONE',  ( -1.000000000000000000, -0.000000000000000000, -0.000000000000000000 ) ) ;
#16715 = CARTESIAN_POINT ( 'NONE',  ( 44.91013252490152752, 64.79948385550240175, 3.727524721679198461 ) ) ;
#16716 = FACE_OUTER_BOUND ( 'NONE', #15456, .T. ) ;
#16717 = B_SPLINE_CURVE_WITH_KNOTS ( 'NONE', 3,
 ( #363, #5239, #9744, #14153, #12400, #9355 ),
 .UNSPECIFIED., .F., .F.,
 ( 4, 2, 4 ),
 ( 0.002365888236227977302, 0.003551327329835078910, 0.004736766423442180518 ),
 .UNSPECIFIED. ) ;
#16718 = DIRECTION ( 'NONE',  ( 1.000000000000000000, 0.000000000000000000, 0.000000000000000000 ) ) ;
#16719 = CARTESIAN_POINT ( 'NONE',  ( 47.37792948025170858, 51.60051614449766788, 7.992620115222797139 ) ) ;
#16720 = ADVANCED_FACE ( 'NONE', ( #17976 ), #10492, .T. ) ;
#16721 = CARTESIAN_POINT ( 'NONE',  ( 51.92680522751238925, 57.40051614449767214, 6.007379884777208190 ) ) ;
#16722 = EDGE_CURVE ( 'NONE', #5652, #8510, #625, .T. ) ;
#16723 = CARTESIAN_POINT ( 'NONE',  ( 50.00000000000000000, 15.00000000000000000, -4.000000000000003553 ) ) ;
#16724 = DIRECTION ( 'NONE',  ( 0.000000000000000000, 0.000000000000000000, -1.000000000000000000 ) ) ;
#16725 = AXIS2_PLACEMENT_3D ( 'NONE', #914, #19176, #7378 ) ;
#16726 = ORIENTED_EDGE ( 'NONE', *, *, #11781, .F. ) ;
#16727 = ORIENTED_EDGE ( 'NONE', *, *, #10749, .F. ) ;
#16728 = CARTESIAN_POINT ( 'NONE',  ( 54.42198456365324688, 44.83981687677464834, -4.999999999999773515 ) ) ;
#16729 = ORIENTED_EDGE ( 'NONE', *, *, #7013, .F. ) ;
#16730 = ADVANCED_FACE ( 'NONE', ( #7752 ), #6270, .T. ) ;
#16731 = DIRECTION ( 'NONE',  ( -0.9768494444668812671, -0.2139279384389642935, 0.000000000000000000 ) ) ;
#16732 = EDGE_CURVE ( 'NONE', #6328, #13819, #1269, .T. ) ;
#16733 = ORIENTED_EDGE ( 'NONE', *, *, #2475, .F. ) ;
#16734 = DIRECTION ( 'NONE',  ( 1.000000000000000000, 0.000000000000000000, 0.000000000000000000 ) ) ;
#16735 = CARTESIAN_POINT ( 'NONE',  ( 49.97728705011488159, 53.49948385550240459, -7.000000000000000888 ) ) ;
#16736 = ADVANCED_FACE ( 'NONE', ( #15113 ), #9697, .T. ) ;
#16737 = ORIENTED_EDGE ( 'NONE', *, *, #3110, .F. ) ;
#16738 = DIRECTION ( 'NONE',  ( 1.000000000000000000, 0.000000000000000000, 0.000000000000000000 ) ) ;
#16739 = EDGE_LOOP ( 'NONE', ( #10581, #17030, #1777, #9497 ) ) ;
#16740 = CARTESIAN_POINT ( 'NONE',  ( 45.27934281921075410, 49.29948385550240886, -6.458785618021043895 ) ) ;
#16741 = DIRECTION ( 'NONE',  ( 0.000000000000000000, 0.000000000000000000, 1.000000000000000000 ) ) ;
#16742 = CARTESIAN_POINT ( 'NONE',  ( 49.97728705011488159, 57.49948385550241170, -7.000000000000000888 ) ) ;
#16743 = CARTESIAN_POINT ( 'NONE',  ( 6.244297270354683960, 1.802013835206515036E-11, 5.105276777067893512 ) ) ;
#16744 = LINE ( 'NONE', #3311, #11182 ) ;
#16745 = CARTESIAN_POINT ( 'NONE',  ( 45.86712807150329496, 55.70051614449766220, 5.649768623646139964 ) ) ;
#16746 = DIRECTION ( 'NONE',  ( -1.000000000000000000, -0.000000000000000000, -0.000000000000000000 ) ) ;
#16747 = CARTESIAN_POINT ( 'NONE',  ( 54.09612160359786515, 49.69948385550240744, -5.676469297603166098 ) ) ;
#16748 = CARTESIAN_POINT ( 'NONE',  ( -7.211304515372548352, -38.65468003441944944, -9.000000000000000000 ) ) ;
#16749 = ORIENTED_EDGE ( 'NONE', *, *, #2942, .T. ) ;
#16750 = VERTEX_POINT ( 'NONE', #14199 ) ;
#16751 = ORIENTED_EDGE ( 'NONE', *, *, #10519, .F. ) ;
#16752 = DIRECTION ( 'NONE',  ( -0.000000000000000000, 1.000000000000000000, 1.224646799147353207E-16 ) ) ;
#16753 = CONICAL_SURFACE ( 'NONE', #452, 5.371010071662833063, 1.221730476396037490 ) ;
#16754 = CARTESIAN_POINT ( 'NONE',  ( 42.63976443033212860, 54.99948385550241170, 0.02388180880522514787 ) ) ;
#16755 = EDGE_LOOP ( 'NONE', ( #19378, #17729, #4190, #9971 ) ) ;
#16756 = CARTESIAN_POINT ( 'NONE',  ( 6.452281807715811723, 5.797857616945992554, -1.918911630784297550E-16 ) ) ;
#16757 = CIRCLE ( 'NONE', #16452, 1.000000000000000222 ) ;
#16758 = VERTEX_POINT ( 'NONE', #17639 ) ;
#16759 = CARTESIAN_POINT ( 'NONE',  ( 54.09612160359792199, 61.30051614449766362, 5.676469297603124353 ) ) ;
#16760 = EDGE_LOOP ( 'NONE', ( #19303, #384 ) ) ;
#16761 = EDGE_CURVE ( 'NONE', #12225, #14264, #18558, .T. ) ;
#16762 = CARTESIAN_POINT ( 'NONE',  ( 0.3198814748697593746, 4.434118497892183264, -0.3507732604232499107 ) ) ;
#16763 = UNCERTAINTY_MEASURE_WITH_UNIT (LENGTH_MEASURE( 1.000000000000000082E-05 ), #18357, 'distance_accuracy_value', 'NONE');
#16764 = CARTESIAN_POINT ( 'NONE',  ( 2.000000000000000000, 0.000000000000000000, 0.000000000000000000 ) ) ;
#16765 = AXIS2_PLACEMENT_3D ( 'NONE', #497, #2070, #6373 ) ;
#16766 = AXIS2_PLACEMENT_3D ( 'NONE', #6, #13620, #4610 ) ;
#16767 = CARTESIAN_POINT ( 'NONE',  ( 46.49166364869456913, 58.30051614449765651, -4.867452303228181343 ) ) ;
#16768 = LINE ( 'NONE', #18250, #17074 ) ;
#16769 = EDGE_CURVE ( 'NONE', #16030, #18044, #6892, .T. ) ;
#16770 = CARTESIAN_POINT ( 'NONE',  ( 0.04320752586819863461, 0.9836842030436160345, 4.999999999999999112 ) ) ;
#16771 = CARTESIAN_POINT ( 'NONE',  ( 55.71335778527780747, 64.09948385550239891, 1.832500667257165983 ) ) ;
#16772 = DIRECTION ( 'NONE',  ( 0.000000000000000000, 0.000000000000000000, 1.000000000000000000 ) ) ;
#16773 = AXIS2_PLACEMENT_3D ( 'NONE', #2064, #8026, #12443 ) ;
#16774 = CARTESIAN_POINT ( 'NONE',  ( 42.38452918213190657, 51.90051614449765793, 2.450534656007115508 ) ) ;
#16775 = ORIENTED_EDGE ( 'NONE', *, *, #12082, .T. ) ;
#16776 = CARTESIAN_POINT ( 'NONE',  ( 2.449293598294706513E-15, -20.00000000000000000, 9.000000000000000000 ) ) ;
#16777 =( LENGTH_UNIT ( ) NAMED_UNIT ( * ) SI_UNIT ( .MILLI., .METRE. ) );
#16778 = ORIENTED_EDGE ( 'NONE', *, *, #9921, .T. ) ;
#16779 = CARTESIAN_POINT ( 'NONE',  ( 3.129923130707922496, -23.63917314727666152, -8.999999999999996447 ) ) ;
#16780 = APPLICATION_PROTOCOL_DEFINITION ( 'draft international standard', 'automotive_design', 1998, #17919 ) ;
#16781 = ORIENTED_EDGE ( 'NONE', *, *, #3792, .T. ) ;
#16782 = DIRECTION ( 'NONE',  ( -0.000000000000000000, 0.000000000000000000, -1.000000000000000000 ) ) ;
#16783 = DIRECTION ( 'NONE',  ( 0.000000000000000000, 0.000000000000000000, 1.000000000000000000 ) ) ;
#16784 = CIRCLE ( 'NONE', #6436, 5.999999999999977796 ) ;
#16785 = DIRECTION ( 'NONE',  ( -0.000000000000000000, -0.000000000000000000, 1.000000000000000000 ) ) ;
#16786 = DIRECTION ( 'NONE',  ( 0.000000000000000000, 0.000000000000000000, 1.000000000000000000 ) ) ;
#16787 = PLANE ( 'NONE',  #15474 ) ;
#16788 = CARTESIAN_POINT ( 'NONE',  ( 2.500000000000000888, 3.061616997868384127E-16, -4.974599999999998801 ) ) ;
#16789 = CIRCLE ( 'NONE', #19000, 1.000000000000001110 ) ;
#16790 = CARTESIAN_POINT ( 'NONE',  ( 46.45491332379572924, 47.29948385550241596, -4.840751629271157874 ) ) ;
#16791 = LINE ( 'NONE', #12559, #14082 ) ;
#16792 = CARTESIAN_POINT ( 'NONE',  ( 54.68390685589033495, 61.69948385550240744, -6.485486291978119766 ) ) ;
#16793 = CARTESIAN_POINT ( 'NONE',  ( 57.36023556966787851, 57.00051614449766646, 0.02388180880515038476 ) ) ;
#16794 = LINE ( 'NONE', #14118, #6191 ) ;
#16795 = CARTESIAN_POINT ( 'NONE',  ( -179.9999999999999716, -14.99999999999999289, 9.000000000000000000 ) ) ;
#16796 = AXIS2_PLACEMENT_3D ( 'NONE', #6933, #12913, #14479 ) ;
#16797 = FILL_AREA_STYLE ('',( #9517 ) ) ;
#16798 = ORIENTED_EDGE ( 'NONE', *, *, #7237, .T. ) ;
#16799 = CIRCLE ( 'NONE', #2722, 24.99999999999999289 ) ;
#16800 = LINE ( 'NONE', #6207, #13448 ) ;
#16801 = CARTESIAN_POINT ( 'NONE',  ( 43.33558569842706021, 47.90051614449765793, 2.141517661632167169 ) ) ;
#16802 = B_SPLINE_CURVE_WITH_KNOTS ( 'NONE', 3,
 ( #3284, #3570, #9246, #4764 ),
 .UNSPECIFIED., .F., .F.,
 ( 4, 4 ),
 ( 0.000000000000000000, 0.002452478801916376308 ),
 .UNSPECIFIED. ) ;
#16803 = DIRECTION ( 'NONE',  ( -1.000000000000000000, 0.000000000000000000, -0.000000000000000000 ) ) ;
#16804 = LINE ( 'NONE', #7774, #9284 ) ;
#16805 = ORIENTED_EDGE ( 'NONE', *, *, #7636, .T. ) ;
#16806 = DIRECTION ( 'NONE',  ( 0.02857142857142857401, -0.9995917534020515305, 0.000000000000000000 ) ) ;
#16807 = VECTOR ( 'NONE', #16582, 1000.000000000000000 ) ;
#16808 = DIRECTION ( 'NONE',  ( 0.8660254037844374864, -0.5000000000000018874, 0.000000000000000000 ) ) ;
#16809 = CARTESIAN_POINT ( 'NONE',  ( 48.02776887271750184, 45.60051614449765367, 5.992620115222795363 ) ) ;
#16810 = CARTESIAN_POINT ( 'NONE',  ( -74.99999999999997158, -39.99999999999998579, 10.00000000000000000 ) ) ;
#16811 = CYLINDRICAL_SURFACE ( 'NONE', #2686, 20.00000000000000000 ) ;
#16812 =( BOUNDED_SURFACE ( )  B_SPLINE_SURFACE ( 3, 2, ( 
 ( #3953, #9914, #10115 ),
 ( #4052, #10014, #2500 ),
 ( #2691, #8454, #13158 ),
 ( #10201, #17685, #1017 ),
 ( #6979, #12959, #19174 ),
 ( #16205, #1308, #7567 ) ),
 .UNSPECIFIED., .F., .F., .F. ) 
 B_SPLINE_SURFACE_WITH_KNOTS ( ( 4, 2, 4 ),
 ( 3, 3 ),
 ( 0.02032853247518126225, 0.02278863295364821212, 0.02524873343211516200 ),
 ( 0.000000000000000000, 1.000000000000000000 ),
 .UNSPECIFIED. ) 
 GEOMETRIC_REPRESENTATION_ITEM ( )  RATIONAL_B_SPLINE_SURFACE ( (
 ( 1.000000000000000000, 0.8047781615896835161, 1.000000000000000000),
 ( 1.000000000000000000, 0.8123767586291043008, 1.000000000000000000),
 ( 1.000000000000000000, 0.8190662415562011134, 1.000000000000000000),
 ( 1.000000000000000000, 0.8192361015671398849, 1.000000000000000000),
 ( 1.000000000000000000, 0.8126135807102121689, 1.000000000000000000),
 ( 1.000000000000000000, 0.8047712338318585568, 1.000000000000000000) ) ) 
 REPRESENTATION_ITEM ( '' )  SURFACE ( )  );
#16813 = CARTESIAN_POINT ( 'NONE',  ( 56.79116909180259398, 61.20051614449766220, 4.963592699178938972 ) ) ;
#16814 = CARTESIAN_POINT ( 'NONE',  ( 44.91013252490150620, 54.20051614449766220, -3.727524721679154940 ) ) ;
#16815 = PLANE ( 'NONE',  #367 ) ;
#16816 = CARTESIAN_POINT ( 'NONE',  ( 1.150000000000001688, 0.000000000000000000, 0.000000000000000000 ) ) ;
#16817 = ORIENTED_EDGE ( 'NONE', *, *, #4125, .T. ) ;
#16818 = VECTOR ( 'NONE', #8574, 1000.000000000000000 ) ;
#16819 = ADVANCED_FACE ( 'NONE', ( #12444 ), #589, .T. ) ;
#16820 = ORIENTED_EDGE ( 'NONE', *, *, #9283, .T. ) ;
#16821 = CARTESIAN_POINT ( 'NONE',  ( 54.89903213687075834, 44.74560054925188268, -5.000000000000007105 ) ) ;
#16822 = TOROIDAL_SURFACE ( 'NONE', #3671, 3.299999999999999822, 0.2000000000000000111 ) ;
#16823 = EDGE_LOOP ( 'NONE', ( #7123, #19358, #5064, #3964 ) ) ;
#16824 = DIRECTION ( 'NONE',  ( 0.000000000000000000, 0.000000000000000000, -1.000000000000000000 ) ) ;
#16825 = ORIENTED_EDGE ( 'NONE', *, *, #19251, .F. ) ;
#16826 = CARTESIAN_POINT ( 'NONE',  ( 2.449293598294706513E-15, -20.00000000000000000, 9.000000000000000000 ) ) ;
#16827 = ADVANCED_FACE ( 'NONE', ( #5655 ), #19114, .T. ) ;
#16828 = CARTESIAN_POINT ( 'NONE',  ( 54.09612160359786515, 51.69948385550240744, -5.676469297603166098 ) ) ;
#16829 = AXIS2_PLACEMENT_3D ( 'NONE', #11974, #8842, #19366 ) ;
#16830 = EDGE_CURVE ( 'NONE', #19111, #5570, #3726, .T. ) ;
#16831 = ORIENTED_EDGE ( 'NONE', *, *, #16258, .F. ) ;
#16832 = DIRECTION ( 'NONE',  ( 0.000000000000000000, -1.000000000000000000, 0.000000000000000000 ) ) ;
#16833 = ORIENTED_EDGE ( 'NONE', *, *, #13526, .T. ) ;
#16834 = CARTESIAN_POINT ( 'NONE',  ( 43.18075615816989199, 49.19948385550240744, -4.924951120819313743 ) ) ;
#16835 = CARTESIAN_POINT ( 'NONE',  ( 4.158921444904715159, -2.089933220600048713, -3.500000000000000000 ) ) ;
#16836 = EDGE_CURVE ( 'NONE', #590, #1122, #17243, .T. ) ;
#16837 = AXIS2_PLACEMENT_3D ( 'NONE', #14686, #7045, #10081 ) ;
#16838 = CARTESIAN_POINT ( 'NONE',  ( 55.08986747509847248, 45.79948385550240886, -3.727524721679197572 ) ) ;
#16839 = CARTESIAN_POINT ( 'NONE',  ( 6.271006797790669829, 0.9853839345309320930, 5.106080050406710313 ) ) ;
#16840 = CONICAL_SURFACE ( 'NONE', #8363, 4.000000000000003553, 1.029744260000001077 ) ;
#16841 = CARTESIAN_POINT ( 'NONE',  ( 56.66441430157294690, 60.90051614449766504, -2.141517661632166281 ) ) ;
#16842 = ADVANCED_FACE ( 'NONE', ( #16984 ), #6464, .F. ) ;
#16843 = EDGE_CURVE ( 'NONE', #15857, #16855, #14404, .T. ) ;
#16844 = CARTESIAN_POINT ( 'NONE',  ( 4.630153689607048761, 6.577590292450083844E-16, 5.371010071662833063 ) ) ;
#16845 = CARTESIAN_POINT ( 'NONE',  ( 52.29715082351547295, 50.39948385550240317, 6.992620115222774047 ) ) ;
#16846 = DIRECTION ( 'NONE',  ( -0.000000000000000000, -0.000000000000000000, 1.000000000000000000 ) ) ;
#16847 = VERTEX_POINT ( 'NONE', #13908 ) ;
#16848 = AXIS2_PLACEMENT_3D ( 'NONE', #8034, #18365, #3452 ) ;
#16849 = ORIENTED_EDGE ( 'NONE', *, *, #9992, .T. ) ;
#16850 = LINE ( 'NONE', #13604, #16263 ) ;
#16851 = SHAPE_REPRESENTATION_RELATIONSHIP ( 'NONE' , 'NONE' ,  #1297, #6165 ) ;
#16852 = CIRCLE ( 'NONE', #16230, 0.2000000000000000944 ) ;
#16853 = CARTESIAN_POINT ( 'NONE',  ( 52.29715082351547295, 50.39948385550240317, 6.992620115222774047 ) ) ;
#16854 = SURFACE_STYLE_USAGE ( .BOTH. , #13883 ) ;
#16855 = VERTEX_POINT ( 'NONE', #784 ) ;
#16856 = CIRCLE ( 'NONE', #4319, 20.00000000000000000 ) ;
#16857 = DIRECTION ( 'NONE',  ( 0.000000000000000000, 0.000000000000000000, 1.000000000000000000 ) ) ;
#16858 = EDGE_CURVE ( 'NONE', #14352, #17307, #493, .T. ) ;
#16859 = EDGE_CURVE ( 'NONE', #8337, #10629, #3538, .T. ) ;
#16860 = VERTEX_POINT ( 'NONE', #9496 ) ;
#16861 = DIRECTION ( 'NONE',  ( 0.000000000000000000, 0.000000000000000000, -1.000000000000000000 ) ) ;
#16862 = ORIENTED_EDGE ( 'NONE', *, *, #18497, .T. ) ;
#16863 = PLANE ( 'NONE',  #662 ) ;
#16864 = FACE_OUTER_BOUND ( 'NONE', #19030, .T. ) ;
#16865 = CARTESIAN_POINT ( 'NONE',  ( 48.07319477248762496, 56.40051614449765793, -6.007379884777208190 ) ) ;
#16866 = FACE_OUTER_BOUND ( 'NONE', #4407, .T. ) ;
#16867 = VECTOR ( 'NONE', #13312, 1000.000000000000000 ) ;
#16868 = LINE ( 'NONE', #3245, #4888 ) ;
#16869 = FACE_OUTER_BOUND ( 'NONE', #8879, .T. ) ;
#16870 = CARTESIAN_POINT ( 'NONE',  ( 54.72065718078918906, 58.70051614449765509, -6.458785618021089192 ) ) ;
#16871 = ORIENTED_EDGE ( 'NONE', *, *, #15736, .F. ) ;
#16872 = ORIENTED_EDGE ( 'NONE', *, *, #1106, .F. ) ;
#16873 = CARTESIAN_POINT ( 'NONE',  ( 32.00000000000000000, -3.000000000000000000, -5.999999999999998224 ) ) ;
#16874 = SURFACE_STYLE_FILL_AREA ( #16585 ) ;
#16875 = ORIENTED_EDGE ( 'NONE', *, *, #9024, .F. ) ;
#16876 = LINE ( 'NONE', #17068, #4993 ) ;
#16877 = APPLICATION_PROTOCOL_DEFINITION ( 'draft international standard', 'automotive_design', 1998, #17284 ) ;
#16878 = ORIENTED_EDGE ( 'NONE', *, *, #18301, .T. ) ;
#16879 = CARTESIAN_POINT ( 'NONE',  ( 6.371919382990606451, -1.972754410575515704, -5.108792907957607099 ) ) ;
#16880 = AXIS2_PLACEMENT_3D ( 'NONE', #9954, #10058, #5454 ) ;
#16881 = EDGE_CURVE ( 'NONE', #9457, #5879, #7127, .T. ) ;
#16882 = VECTOR ( 'NONE', #12907, 1000.000000000000000 ) ;
#16883 = PLANE ( 'NONE',  #14714 ) ;
#16884 = ADVANCED_FACE ( 'NONE', ( #9691, #13104 ), #15690, .T. ) ;
#16885 = EDGE_CURVE ( 'NONE', #3214, #16273, #6568, .T. ) ;
#16886 = CARTESIAN_POINT ( 'NONE',  ( 49.97728705011488159, 63.49948385550241170, -7.000000000000000888 ) ) ;
#16887 = CARTESIAN_POINT ( 'NONE',  ( -19.99999999999999289, -14.99999999999998579, -23.00000000000000000 ) ) ;
#16888 = CARTESIAN_POINT ( 'NONE',  ( 0.1999999999999985678, -6.997142273814360713, -0.8000000000000000444 ) ) ;
#16889 = DIRECTION ( 'NONE',  ( 0.000000000000000000, 0.000000000000000000, -1.000000000000000000 ) ) ;
#16890 = CARTESIAN_POINT ( 'NONE',  ( 54.09612160359786515, 61.69948385550240744, -5.676469297603166098 ) ) ;
#16891 = LINE ( 'NONE', #3454, #11579 ) ;
#16892 = CARTESIAN_POINT ( 'NONE',  ( 58.41169779390614281, 59.99948385550241170, -0.02388180880523160798 ) ) ;
#16893 = AXIS2_PLACEMENT_3D ( 'NONE', #12910, #8391, #4091 ) ;
#16894 = CARTESIAN_POINT ( 'NONE',  ( 55.96859303347802239, 60.80051614449764941, -4.306917132069484566 ) ) ;
#16895 = CIRCLE ( 'NONE', #15007, 20.00000000000000000 ) ;
#16896 = FACE_OUTER_BOUND ( 'NONE', #5448, .T. ) ;
#16897 = CARTESIAN_POINT ( 'NONE',  ( -1.250000000000001110, 0.000000000000000000, 0.000000000000000000 ) ) ;
#16898 = ADVANCED_FACE ( 'NONE', ( #8127 ), #18737, .F. ) ;
#16899 = PRESENTATION_LAYER_ASSIGNMENT (  '', '', ( #14055 ) ) ;
#16900 = ORIENTED_EDGE ( 'NONE', *, *, #12646, .T. ) ;
#16901 = ADVANCED_FACE ( 'NONE', ( #6562 ), #9589, .T. ) ;
#16902 = CARTESIAN_POINT ( 'NONE',  ( 6.367873360227556567, 2.886751345948123770, -5.000000000000000000 ) ) ;
#16903 = CARTESIAN_POINT ( 'NONE',  ( 43.34962307344078880, 46.10051614449766078, -2.184720259617096705 ) ) ;
#16904 = VECTOR ( 'NONE', #12203, 1000.000000000000000 ) ;
#16905 = CARTESIAN_POINT ( 'NONE',  ( 49.97728705011488159, 61.49948385550240459, -7.000000000000000888 ) ) ;
#16906 = CARTESIAN_POINT ( 'NONE',  ( -19.02113032590308705, -13.81966011250110249, -9.000000000000000000 ) ) ;
#16907 = EDGE_LOOP ( 'NONE', ( #9347, #2899, #13515, #14057 ) ) ;
#16908 = CARTESIAN_POINT ( 'NONE',  ( 10.93224627749286526, -3.252283996668575483, -9.000000000000000000 ) ) ;
#16909 = DIRECTION ( 'NONE',  ( 1.000000000000000000, 0.000000000000000000, 0.000000000000000000 ) ) ;
#16910 = CARTESIAN_POINT ( 'NONE',  ( 53.50833635130540955, 61.69948385550240744, -4.867452303228209765 ) ) ;
#16911 = CARTESIAN_POINT ( 'NONE',  ( -5.130877905917148318, -39.33065161639853358, 9.000000000000000000 ) ) ;
#16912 = VECTOR ( 'NONE', #8538, 1000.000000000000000 ) ;
#16913 = CARTESIAN_POINT ( 'NONE',  ( 3.973110223767137850, -2.261493176400255405E-11, -3.565797985667433334 ) ) ;
#16914 = CARTESIAN_POINT ( 'NONE',  ( 56.79116909180259398, 59.20051614449766220, 4.963592699178938972 ) ) ;
#16915 = CARTESIAN_POINT ( 'NONE',  ( 48.07319477248762496, 62.40051614449765793, -6.007379884777208190 ) ) ;
#16916 = DIRECTION ( 'NONE',  ( -0.000000000000000000, 1.345283343056720273E-15, 1.000000000000000000 ) ) ;
#16917 = DIRECTION ( 'NONE',  ( 1.000000000000000000, 0.000000000000000000, 0.000000000000000000 ) ) ;
#16918 = VECTOR ( 'NONE', #16592, 1000.000000000000000 ) ;
#16919 = VERTEX_POINT ( 'NONE', #17270 ) ;
#16920 = VERTEX_POINT ( 'NONE', #5953 ) ;
#16921 = CARTESIAN_POINT ( 'NONE',  ( -22.14999999999999858, -19.99999999999999289, -23.00000000000000000 ) ) ;
#16922 = VERTEX_POINT ( 'NONE', #9072 ) ;
#16923 = LINE ( 'NONE', #6414, #599 ) ;
#16924 = CIRCLE ( 'NONE', #10651, 0.5155456020628804703 ) ;
#16925 = ORIENTED_EDGE ( 'NONE', *, *, #265, .T. ) ;
#16926 = CARTESIAN_POINT ( 'NONE',  ( -65.14999999999996305, 32.50000000000001421, -15.00000000000000000 ) ) ;
#16927 = CARTESIAN_POINT ( 'NONE',  ( 45.90387839640214196, 52.69948385550240033, 5.676469297603166098 ) ) ;
#16928 = VERTEX_POINT ( 'NONE', #7608 ) ;
#16929 = PLANE ( 'NONE',  #14444 ) ;
#16930 = ORIENTED_EDGE ( 'NONE', *, *, #9681, .T. ) ;
#16931 = CARTESIAN_POINT ( 'NONE',  ( 57.61547081786812896, 52.09948385550241312, 2.450534656007040901 ) ) ;
#16932 = VECTOR ( 'NONE', #2272, 1000.000000000000000 ) ;
#16933 = DIRECTION ( 'NONE',  ( 1.000000000000000000, 0.000000000000000000, 0.000000000000000000 ) ) ;
#16934 = CARTESIAN_POINT ( 'NONE',  ( 44.05948171654949874, 64.79948385550240175, 4.345558710429105354 ) ) ;
#16935 = DIRECTION ( 'NONE',  ( -0.000000000000000000, -0.000000000000000000, -1.000000000000000000 ) ) ;
#16936 = FACE_OUTER_BOUND ( 'NONE', #6783, .T. ) ;
#16937 = VECTOR ( 'NONE', #15574, 1000.000000000000000 ) ;
#16938 = CIRCLE ( 'NONE', #8775, 4.799999999999999822 ) ;
#16939 = CARTESIAN_POINT ( 'NONE',  ( 44.03140696652198471, 63.80051614449765651, 4.306917132069485454 ) ) ;
#16940 = CARTESIAN_POINT ( 'NONE',  ( -2.354826896168714434, -6.962563485461402024, 0.000000000000000000 ) ) ;
#16941 = AXIS2_PLACEMENT_3D ( 'NONE', #2407, #3960, #18781 ) ;
#16942 = CARTESIAN_POINT ( 'NONE',  ( 44.05948171654949874, 60.79948385550240886, 4.345558710429105354 ) ) ;
#16943 = CARTESIAN_POINT ( 'NONE',  ( 6.518095160331716542, -5.866179305615093931, 2.176274696337492837E-17 ) ) ;
#16944 = EDGE_CURVE ( 'NONE', #18044, #15181, #10963, .T. ) ;
#16945 = EDGE_LOOP ( 'NONE', ( #1674, #835, #2311, #7195 ) ) ;
#16946 = ORIENTED_EDGE ( 'NONE', *, *, #4975, .T. ) ;
#16947 = CARTESIAN_POINT ( 'NONE',  ( -154.9999999999999716, -14.99999999999999645, -4.000000000000000000 ) ) ;
#16948 =( NAMED_UNIT ( * ) SI_UNIT ( $, .STERADIAN. ) SOLID_ANGLE_UNIT ( ) );
#16949 = AXIS2_PLACEMENT_3D ( 'NONE', #882, #14007, #18560 ) ;
#16950 = EDGE_CURVE ( 'NONE', #1126, #9852, #5326, .T. ) ;
#16951 = CARTESIAN_POINT ( 'NONE',  ( 42.63976443033212860, 52.99948385550240459, 0.02388180880522514787 ) ) ;
#16952 = DIRECTION ( 'NONE',  ( -9.858538378746663627E-23, 5.031452844637890958E-23, -1.000000000000000000 ) ) ;
#16953 = CIRCLE ( 'NONE', #973, 2.500000000000000444 ) ;
#16954 = ORIENTED_EDGE ( 'NONE', *, *, #7876, .F. ) ;
#16955 = AXIS2_PLACEMENT_3D ( 'NONE', #15625, #15922, #2507 ) ;
#16956 = CARTESIAN_POINT ( 'NONE',  ( 0.000000000000000000, -3.031088913245534755, -1.750000000000001332 ) ) ;
#16957 = EDGE_CURVE ( 'NONE', #468, #3703, #7418, .T. ) ;
#16958 = ADVANCED_FACE ( 'NONE', ( #13585 ), #7513, .F. ) ;
#16959 = EDGE_LOOP ( 'NONE', ( #14930, #6235, #13582, #2749 ) ) ;
#16960 = CARTESIAN_POINT ( 'NONE',  ( 4.158233816355333623, -39.56295201467608535, 9.000000000000000000 ) ) ;
#16961 = ORIENTED_EDGE ( 'NONE', *, *, #6305, .T. ) ;
#16962 = EDGE_CURVE ( 'NONE', #10892, #8318, #8134, .T. ) ;
#16963 = CARTESIAN_POINT ( 'NONE',  ( 54.09612160359786515, 45.69948385550240744, -5.676469297603166098 ) ) ;
#16964 = UNCERTAINTY_MEASURE_WITH_UNIT (LENGTH_MEASURE( 1.000000000000000082E-05 ), #13852, 'distance_accuracy_value', 'NONE');
#16965 = DIRECTION ( 'NONE',  ( -0.000000000000000000, -0.000000000000000000, 1.000000000000000000 ) ) ;
#16966 = CARTESIAN_POINT ( 'NONE',  ( 51.92680522751238925, 61.40051614449765793, 6.007379884777208190 ) ) ;
#16967 = CARTESIAN_POINT ( 'NONE',  ( -154.9999999999999716, -14.99999999999999645, -15.79999999999999893 ) ) ;
#16968 = PLANE ( 'NONE',  #12702 ) ;
#16969 = CARTESIAN_POINT ( 'NONE',  ( -62.49999999999997158, 32.50000000000001421, 9.999999999999998224 ) ) ;
#16970 = CIRCLE ( 'NONE', #8502, 2.000000000000000000 ) ;
#16971 = AXIS2_PLACEMENT_3D ( 'NONE', #4338, #16602, #217 ) ;
#16972 = EDGE_CURVE ( 'NONE', #17065, #2854, #3463, .T. ) ;
#16973 = CARTESIAN_POINT ( 'NONE',  ( 43.20883090819742023, 60.20051614449766220, -4.963592699178938972 ) ) ;
#16974 = CIRCLE ( 'NONE', #1632, 0.7499999999999997780 ) ;
#16975 = EDGE_CURVE ( 'NONE', #13385, #4387, #8692, .T. ) ;
#16976 = ORIENTED_EDGE ( 'NONE', *, *, #3457, .T. ) ;
#16977 = ORIENTED_EDGE ( 'NONE', *, *, #10347, .T. ) ;
#16978 = DIRECTION ( 'NONE',  ( -9.858538378746663627E-23, 5.031452844637890958E-23, -1.000000000000000000 ) ) ;
#16979 = PRESENTATION_STYLE_ASSIGNMENT (( #9401 ) ) ;
#16980 = B_SPLINE_CURVE_WITH_KNOTS ( 'NONE', 3,
 ( #3662, #8161, #7967, #2302, #11007, #11294, #12120, #7620 ),
 .UNSPECIFIED., .F., .F.,
 ( 4, 2, 2, 4 ),
 ( 2.465131517071352357E-07, 0.001183067374689843057, 0.001774477805458910071, 0.002365888236227977302 ),
 .UNSPECIFIED. ) ;
#16981 = PRODUCT_CONTEXT ( 'NONE', #18288, 'mechanical' ) ;
#16982 = ORIENTED_EDGE ( 'NONE', *, *, #7250, .T. ) ;
#16983 = DIRECTION ( 'NONE',  ( 1.000000000000000000, 0.000000000000000000, 0.000000000000000000 ) ) ;
#16984 = FACE_OUTER_BOUND ( 'NONE', #12808, .T. ) ;
#16985 = ORIENTED_EDGE ( 'NONE', *, *, #15311, .F. ) ;
#16986 = CARTESIAN_POINT ( 'NONE',  ( 1.925929944387235853E-31, 15.00000000000001599, 9.999999999999998224 ) ) ;
#16987 = AXIS2_PLACEMENT_3D ( 'NONE', #5907, #17885, #4449 ) ;
#16988 = UNCERTAINTY_MEASURE_WITH_UNIT (LENGTH_MEASURE( 1.000000000000000082E-05 ), #19323, 'distance_accuracy_value', 'NONE');
#16989 = DIRECTION ( 'NONE',  ( -0.000000000000000000, -0.000000000000000000, 1.000000000000000000 ) ) ;
#16990 = DIRECTION ( 'NONE',  ( -0.000000000000000000, -0.000000000000000000, 1.000000000000000000 ) ) ;
#16991 = DIRECTION ( 'NONE',  ( -0.000000000000000000, -0.000000000000000000, 1.000000000000000000 ) ) ;
#16992 = CARTESIAN_POINT ( 'NONE',  ( 47.74827507625478518, 64.59948385550239891, 7.007379884777227730 ) ) ;
#16993 = DIRECTION ( 'NONE',  ( 1.000000000000000000, 0.000000000000000000, 0.000000000000000000 ) ) ;
#16994 = CARTESIAN_POINT ( 'NONE',  ( 50.02271294988513972, 58.49948385550241170, 8.000000000000001776 ) ) ;
#16995 = CARTESIAN_POINT ( 'NONE',  ( 45.90387839640208512, 60.30051614449766362, -5.676469297603124353 ) ) ;
#16996 = DIRECTION ( 'NONE',  ( 1.000000000000000000, 0.000000000000000000, 0.000000000000000000 ) ) ;
#16997 = DIRECTION ( 'NONE',  ( -0.000000000000000000, -0.000000000000000000, 1.000000000000000000 ) ) ;
#16998 = SURFACE_SIDE_STYLE ('',( #13923 ) ) ;
#16999 = ORIENTED_EDGE ( 'NONE', *, *, #10319, .T. ) ;
#17000 = CARTESIAN_POINT ( 'NONE',  ( 1.925929944387235853E-31, 15.00000000000001599, -15.00000000000000000 ) ) ;
#17001 = CARTESIAN_POINT ( 'NONE',  ( -20.63749999999999574, 0.000000000000000000, 0.000000000000000000 ) ) ;
#17002 = DIRECTION ( 'NONE',  ( 0.000000000000000000, 0.000000000000000000, 1.000000000000000000 ) ) ;
#17003 = CARTESIAN_POINT ( 'NONE',  ( 51.03999344061968912, 45.00000000000002132, -7.500000000000003553 ) ) ;
#17004 = FACE_OUTER_BOUND ( 'NONE', #16175, .T. ) ;
#17005 = ORIENTED_EDGE ( 'NONE', *, *, #7171, .F. ) ;
#17006 = LINE ( 'NONE', #811, #5843 ) ;
#17007 = CARTESIAN_POINT ( 'NONE',  ( 1.000000000000000000, -14.00000000000000000, -9.000000000000001776 ) ) ;
#17008 = EDGE_CURVE ( 'NONE', #2212, #12707, #5402, .T. ) ;
#17009 = CARTESIAN_POINT ( 'NONE',  ( 44.28664221472220675, 61.09948385550241312, -1.832500667257165317 ) ) ;
#17010 = B_SPLINE_CURVE_WITH_KNOTS ( 'NONE', 3,
 ( #17173, #3636, #499, #2174, #4913, #10786, #12356, #15594 ),
 .UNSPECIFIED., .F., .F.,
 ( 4, 2, 2, 4 ),
 ( 0.000000000000000000, 0.002450665683189818828, 0.003675998524784728459, 0.004901331366379638524 ),
 .UNSPECIFIED. ) ;
#17011 = CARTESIAN_POINT ( 'NONE',  ( -54.99999999999996447, -14.99999999999998579, 15.00000000000000000 ) ) ;
#17012 = CARTESIAN_POINT ( 'NONE',  ( 54.09612160359786515, 45.69948385550240744, -5.676469297603166098 ) ) ;
#17013 = DIRECTION ( 'NONE',  ( 0.000000000000000000, 0.000000000000000000, 1.000000000000000000 ) ) ;
#17014 = CARTESIAN_POINT ( 'NONE',  ( 4.050880675075948290, -1.379097446046192665, -3.567934390854430315 ) ) ;
#17015 = CARTESIAN_POINT ( 'NONE',  ( 56.81924384183006538, 62.80051614449766362, -4.924951120819380357 ) ) ;
#17016 = EDGE_CURVE ( 'NONE', #2111, #16399, #1784, .T. ) ;
#17017 = CARTESIAN_POINT ( 'NONE',  ( 55.08986747509849380, 59.20051614449766220, 3.727524721679155384 ) ) ;
#17018 = LINE ( 'NONE', #16723, #5041 ) ;
#17019 = FACE_OUTER_BOUND ( 'NONE', #10818, .T. ) ;
#17020 = EDGE_LOOP ( 'NONE', ( #17236, #19314, #956, #13200 ) ) ;
#17021 = ORIENTED_EDGE ( 'NONE', *, *, #12145, .T. ) ;
#17022 = DIRECTION ( 'NONE',  ( -1.000000000000000000, 0.000000000000000000, 0.000000000000000000 ) ) ;
#17023 = ORIENTED_EDGE ( 'NONE', *, *, #16732, .T. ) ;
#17024 = CARTESIAN_POINT ( 'NONE',  ( 4.050823680195226650, -3.779313952391382792, 0.5899027668435167238 ) ) ;
#17025 = ORIENTED_EDGE ( 'NONE', *, *, #13755, .T. ) ;
#17026 = CARTESIAN_POINT ( 'NONE',  ( -0.1713913650100259145, 0.000000000000000000, 0.000000000000000000 ) ) ;
#17027 = CARTESIAN_POINT ( 'NONE',  ( 44.03140696652193498, 51.19948385550240033, -4.306917132069424170 ) ) ;
#17028 = VERTEX_POINT ( 'NONE', #9025 ) ;
#17029 = CARTESIAN_POINT ( 'NONE',  ( 6.527192678185835817, -2.941622124011024297, -5.095038975456044561 ) ) ;
#17030 = ORIENTED_EDGE ( 'NONE', *, *, #6064, .F. ) ;
#17031 = CARTESIAN_POINT ( 'NONE',  ( 43.20883090819745576, 50.79948385550240175, 4.963592699179006473 ) ) ;
#17032 = CARTESIAN_POINT ( 'NONE',  ( 4.052416734886645777, -1.393505408945131308, -3.567979131523694836 ) ) ;
#17033 = CARTESIAN_POINT ( 'NONE',  ( 53.50833635130540955, 45.69948385550240033, -4.867452303228209765 ) ) ;
#17034 = CARTESIAN_POINT ( 'NONE',  ( 4.093692494532774617, 2.021783646005766322, -3.501831996793843160 ) ) ;
#17035 = DIRECTION ( 'NONE',  ( 0.000000000000000000, 0.000000000000000000, 1.000000000000000000 ) ) ;
#17036 = CARTESIAN_POINT ( 'NONE',  ( 54.13287192849671214, 60.70051614449766220, -5.649768623646139964 ) ) ;
#17037 = CARTESIAN_POINT ( 'NONE',  ( 44.03140696652192787, 59.19948385550238612, -4.306917132069425058 ) ) ;
#17038 = CARTESIAN_POINT ( 'NONE',  ( -158.7997795378487353, -15.04093242902330907, -15.79999999999999893 ) ) ;
#17039 = CARTESIAN_POINT ( 'NONE',  ( -1.250000000000000000, -6.429618962271402616, -1.000000000000000000 ) ) ;
#17040 = EDGE_LOOP ( 'NONE', ( #18090, #10779 ) ) ;
#17041 = ORIENTED_EDGE ( 'NONE', *, *, #17698, .T. ) ;
#17042 = CARTESIAN_POINT ( 'NONE',  ( -19.02113032590304442, -26.18033988749903074, -9.000000000000000000 ) ) ;
#17043 =( NAMED_UNIT ( * ) SI_UNIT ( $, .STERADIAN. ) SOLID_ANGLE_UNIT ( ) );
#17044 = CIRCLE ( 'NONE', #2008, 2.000000000000001332 ) ;
#17045 = CARTESIAN_POINT ( 'NONE',  ( 55.94051828345050836, 51.79948385550240175, -4.345558710429104465 ) ) ;
#17046 = CYLINDRICAL_SURFACE ( 'NONE', #8093, 1.000000000000000888 ) ;
#17047 = ORIENTED_EDGE ( 'NONE', *, *, #3110, .T. ) ;
#17048 = EDGE_LOOP ( 'NONE', ( #6552, #18982, #16034, #15936 ) ) ;
#17049 = CIRCLE ( 'NONE', #8582, 5.000000000000007994 ) ;
#17050 = DIRECTION ( 'NONE',  ( -0.03668796685672144620, 0.9993267699245927949, 2.695122805014889898E-17 ) ) ;
#17051 = ORIENTED_EDGE ( 'NONE', *, *, #9160, .T. ) ;
#17052 = LINE ( 'NONE', #8010, #17891 ) ;
#17053 = ORIENTED_EDGE ( 'NONE', *, *, #16220, .F. ) ;
#17054 = EDGE_CURVE ( 'NONE', #15436, #11089, #18821, .T. ) ;
#17055 = B_SPLINE_CURVE_WITH_KNOTS ( 'NONE', 3,
 ( #12868, #1573, #4311, #5987, #7446, #1372 ),
 .UNSPECIFIED., .F., .F.,
 ( 4, 2, 4 ),
 ( 0.002044882221487539717, 0.003063384235218500652, 0.004081886248949461587 ),
 .UNSPECIFIED. ) ;
#17056 = CARTESIAN_POINT ( 'NONE',  ( 47.70284917648453415, 47.39948385550238896, -6.992620115222774047 ) ) ;
#17057 = CARTESIAN_POINT ( 'NONE',  ( 4.000000000000000000, 2.309401076758515803, -0.4999999999999995559 ) ) ;
#17058 = PRODUCT_DEFINITION ( 'UNKNOWN', '', #14167, #11049 ) ;
#17059 = CARTESIAN_POINT ( 'NONE',  ( 53.50833635130544508, 61.30051614449766362, 4.867452303228181343 ) ) ;
#17060 = DIRECTION ( 'NONE',  ( 1.000000000000000000, 0.000000000000000000, 0.000000000000000000 ) ) ;
#17061 =( NAMED_UNIT ( * ) PLANE_ANGLE_UNIT ( ) SI_UNIT ( $, .RADIAN. ) );
#17062 = DIRECTION ( 'NONE',  ( -1.000000000000000000, -0.000000000000000000, -0.000000000000000000 ) ) ;
#17063 = AXIS2_PLACEMENT_3D ( 'NONE', #9132, #5902, #11870 ) ;
#17064 = CARTESIAN_POINT ( 'NONE',  ( 43.18075615816994173, 59.80051614449766362, 4.924951120819380357 ) ) ;
#17065 = VERTEX_POINT ( 'NONE', #15013 ) ;
#17066 = ORIENTED_EDGE ( 'NONE', *, *, #6636, .T. ) ;
#17067 = CARTESIAN_POINT ( 'NONE',  ( -30.00000000000000000, -40.00000000000000000, 12.50000000000000000 ) ) ;
#17068 = CARTESIAN_POINT ( 'NONE',  ( 62.49999999999998579, 45.00000000000001421, 15.00000000000000000 ) ) ;
#17069 = ADVANCED_FACE ( 'NONE', ( #1490 ), #4819, .F. ) ;
#17070 = VERTEX_POINT ( 'NONE', #7564 ) ;
#17071 = DIRECTION ( 'NONE',  ( 1.000000000000000000, 0.000000000000000000, 0.000000000000000000 ) ) ;
#17072 = DIRECTION ( 'NONE',  ( 1.000000000000000000, 0.000000000000000000, 0.000000000000000000 ) ) ;
#17073 = EDGE_LOOP ( 'NONE', ( #851, #5456, #11883, #14734 ) ) ;
#17074 = VECTOR ( 'NONE', #392, 1000.000000000000000 ) ;
#17075 = EDGE_CURVE ( 'NONE', #8220, #16030, #8771, .T. ) ;
#17076 = DIRECTION ( 'NONE',  ( -1.000000000000000000, 0.000000000000000000, 0.000000000000000000 ) ) ;
#17077 = EDGE_CURVE ( 'NONE', #12235, #8949, #3151, .T. ) ;
#17078 = CARTESIAN_POINT ( 'NONE',  ( 0.000000000000000000, 0.000000000000000000, -0.8000000000000000444 ) ) ;
#17079 = DIRECTION ( 'NONE',  ( 1.000000000000000000, 0.000000000000000000, 0.000000000000000000 ) ) ;
#17080 = MECHANICAL_DESIGN_GEOMETRIC_PRESENTATION_REPRESENTATION (  '', ( #4853 ), #3920 ) ;
#17081 = CARTESIAN_POINT ( 'NONE',  ( 1.925929944387235853E-31, 15.00000000000001599, 15.00000000000000000 ) ) ;
#17082 = CARTESIAN_POINT ( 'NONE',  ( 50.02271294988511841, 46.49948385550240459, 6.000000000000000888 ) ) ;
#17083 = CARTESIAN_POINT ( 'NONE',  ( -12.54977455159125377, -4.427487078052159575, -9.000000000000000000 ) ) ;
#17084 = CARTESIAN_POINT ( 'NONE',  ( 50.02271294988513972, 60.49948385550240459, 8.000000000000001776 ) ) ;
#17085 = CARTESIAN_POINT ( 'NONE',  ( 52.25172492374527877, 63.40051614449765793, 7.007379884777203749 ) ) ;
#17086 = ADVANCED_FACE ( 'NONE', ( #2169 ), #17553, .T. ) ;
#17087 = CYLINDRICAL_SURFACE ( 'NONE', #3700, 2.649999999999985700 ) ;
#17088 =( LENGTH_UNIT ( ) NAMED_UNIT ( * ) SI_UNIT ( .MILLI., .METRE. ) );
#17089 = EDGE_LOOP ( 'NONE', ( #2058, #17051, #19188, #13561 ) ) ;
#17090 = SURFACE_STYLE_USAGE ( .BOTH. , #5114 ) ;
#17091 = AXIS2_PLACEMENT_3D ( 'NONE', #586, #6662, #878 ) ;
#17092 = FACE_OUTER_BOUND ( 'NONE', #12781, .T. ) ;
#17093 = CARTESIAN_POINT ( 'NONE',  ( 52.25172492374528588, 45.40051614449766504, 7.007379884777204637 ) ) ;
#17094 = DIRECTION ( 'NONE',  ( 1.000000000000000000, 0.000000000000000000, 0.000000000000000000 ) ) ;
#17095 = VECTOR ( 'NONE', #8517, 1000.000000000000000 ) ;
#17096 = ADVANCED_FACE ( 'NONE', ( #9499 ), #8131, .T. ) ;
#17097 = CARTESIAN_POINT ( 'NONE',  ( -3.734041964264191549, -23.01611183630746638, -8.999999999999996447 ) ) ;
#17098 = VERTEX_POINT ( 'NONE', #8030 ) ;
#17099 = DIRECTION ( 'NONE',  ( 1.000000000000000000, 0.000000000000000000, 0.000000000000000000 ) ) ;
#17100 = DIRECTION ( 'NONE',  ( -0.000000000000000000, -0.000000000000000000, 1.000000000000000000 ) ) ;
#17101 = DIRECTION ( 'NONE',  ( 1.000000000000000000, 0.000000000000000000, 0.000000000000000000 ) ) ;
#17102 = SURFACE_STYLE_USAGE ( .BOTH. , #15423 ) ;
#17103 = DIRECTION ( 'NONE',  ( 0.000000000000000000, 0.000000000000000000, 1.000000000000000000 ) ) ;
#17104 = CARTESIAN_POINT ( 'NONE',  ( 50.02271294988505446, 62.50051614449767357, -8.000000000000001776 ) ) ;
#17105 = VECTOR ( 'NONE', #2941, 1000.000000000000000 ) ;
#17106 = CARTESIAN_POINT ( 'NONE',  ( 44.91013252490150620, 62.20051614449766220, -3.727524721679154940 ) ) ;
#17107 = CARTESIAN_POINT ( 'NONE',  ( 2.000000000000000000, 0.8865213383406715941, 1.535499999999999199 ) ) ;
#17108 = CARTESIAN_POINT ( 'NONE',  ( 6.357987042335720318, 1.995285544161303992, 5.108766985362874102 ) ) ;
#17109 = ORIENTED_EDGE ( 'NONE', *, *, #3762, .F. ) ;
#17110 = VECTOR ( 'NONE', #10573, 1000.000000000000000 ) ;
#17111 = ORIENTED_EDGE ( 'NONE', *, *, #6051, .F. ) ;
#17112 = DIRECTION ( 'NONE',  ( 1.000000000000000000, 0.000000000000000000, 0.000000000000000000 ) ) ;
#17113 = VERTEX_POINT ( 'NONE', #5002 ) ;
#17114 = EDGE_CURVE ( 'NONE', #8527, #5177, #18741, .T. ) ;
#17115 = CARTESIAN_POINT ( 'NONE',  ( -4.000000000000000000, 2.309401076758498483, -0.4999999999999927280 ) ) ;
#17116 = VERTEX_POINT ( 'NONE', #18652 ) ;
#17117 = CARTESIAN_POINT ( 'NONE',  ( 1.925929944387235853E-31, 15.00000000000001599, -9.999999999999998224 ) ) ;
#17118 = EDGE_CURVE ( 'NONE', #11964, #15631, #694, .T. ) ;
#17119 = CARTESIAN_POINT ( 'NONE',  ( 52.29715082351547295, 60.39948385550240317, 6.992620115222774047 ) ) ;
#17120 = ORIENTED_EDGE ( 'NONE', *, *, #2455, .T. ) ;
#17121 = FACE_OUTER_BOUND ( 'NONE', #7152, .T. ) ;
#17122 = ORIENTED_EDGE ( 'NONE', *, *, #18452, .F. ) ;
#17123 = CARTESIAN_POINT ( 'NONE',  ( 43.20883090819745576, 52.79948385550240175, 4.963592699179006473 ) ) ;
#17124 = LINE ( 'NONE', #14059, #12950 ) ;
#17125 = PRODUCT_DEFINITION_SHAPE ( 'NONE', 'NONE',  #5304 ) ;
#17126 = CARTESIAN_POINT ( 'NONE',  ( 54.13287192849676188, 62.29948385550240886, 5.649768623646098220 ) ) ;
#17127 = LINE ( 'NONE', #2229, #4473 ) ;
#17128 = CARTESIAN_POINT ( 'NONE',  ( -65.14999999999996305, 32.50000000000001421, -9.999999999999998224 ) ) ;
#17129 = CARTESIAN_POINT ( 'NONE',  ( 52.29715082351538769, 60.60051614449764656, -6.992620115222796251 ) ) ;
#17130 = CARTESIAN_POINT ( 'NONE',  ( 53.54508667620428497, 62.29948385550241596, 4.840751629271157874 ) ) ;
#17131 = CARTESIAN_POINT ( 'NONE',  ( 55.94051828345050836, 57.79948385550238754, -4.345558710429104465 ) ) ;
#17132 = CARTESIAN_POINT ( 'NONE',  ( 3.510273485745307731, 2.827716139362654424, -3.610536846335885564 ) ) ;
#17133 = CARTESIAN_POINT ( 'NONE',  ( 2.000000000000000000, -6.429618962271402616, 0.000000000000000000 ) ) ;
#17134 = ORIENTED_EDGE ( 'NONE', *, *, #15736, .T. ) ;
#17135 = VERTEX_POINT ( 'NONE', #8325 ) ;
#17136 = DIRECTION ( 'NONE',  ( 0.000000000000000000, 1.224646799147351975E-16, 1.000000000000000000 ) ) ;
#17137 = SURFACE_STYLE_USAGE ( .BOTH. , #3895 ) ;
#17138 = EDGE_CURVE ( 'NONE', #1462, #9490, #642, .T. ) ;
#17139 = CIRCLE ( 'NONE', #8669, 5.371010071662833063 ) ;
#17140 = CARTESIAN_POINT ( 'NONE',  ( 55.96859303347804371, 54.19948385550240033, 4.306917132069425946 ) ) ;
#17141 = LINE ( 'NONE', #13005, #1220 ) ;
#17142 = EDGE_LOOP ( 'NONE', ( #11359, #17320, #12527 ) ) ;
#17143 = ORIENTED_EDGE ( 'NONE', *, *, #9097, .F. ) ;
#17144 = CARTESIAN_POINT ( 'NONE',  ( 0.2174200650117580902, -3.876582599186216616, -0.2855619784720681564 ) ) ;
#17145 = VERTEX_POINT ( 'NONE', #5288 ) ;
#17146 = DIRECTION ( 'NONE',  ( -1.000000000000000000, 1.734723475976807094E-16, 0.000000000000000000 ) ) ;
#17147 = ORIENTED_EDGE ( 'NONE', *, *, #9150, .F. ) ;
#17148 = CARTESIAN_POINT ( 'NONE',  ( 54.13287192849676188, 46.29948385550240886, 5.649768623646098220 ) ) ;
#17149 = LINE ( 'NONE', #4002, #19354 ) ;
#17150 = CARTESIAN_POINT ( 'NONE',  ( 51.92680522751238925, 63.40051614449765083, 6.007379884777208190 ) ) ;
#17151 = DIRECTION ( 'NONE',  ( 0.000000000000000000, 0.000000000000000000, -1.000000000000000000 ) ) ;
#17152 = DIRECTION ( 'NONE',  ( -1.000000000000000000, 0.000000000000000000, 0.000000000000000000 ) ) ;
#17153 = DIRECTION ( 'NONE',  ( 0.000000000000000000, 0.000000000000000000, 1.000000000000000000 ) ) ;
#17154 = AXIS2_PLACEMENT_3D ( 'NONE', #12071, #10596, #6102 ) ;
#17155 = CARTESIAN_POINT ( 'NONE',  ( 54.68390685589039890, 61.30051614449766362, 6.485486291978072693 ) ) ;
#17156 = VECTOR ( 'NONE', #2779, 1000.000000000000000 ) ;
#17157 = EDGE_LOOP ( 'NONE', ( #1705, #12975, #8895, #8219 ) ) ;
#17158 = ORIENTED_EDGE ( 'NONE', *, *, #10711, .F. ) ;
#17159 = LINE ( 'NONE', #11546, #4023 ) ;
#17160 = FILL_AREA_STYLE_COLOUR ( '', #14339 ) ;
#17161 =( GEOMETRIC_REPRESENTATION_CONTEXT ( 3 ) GLOBAL_UNCERTAINTY_ASSIGNED_CONTEXT ( ( #9500 ) ) GLOBAL_UNIT_ASSIGNED_CONTEXT ( ( #7803, #13782, #372 ) ) REPRESENTATION_CONTEXT ( 'NONE', 'WORKASPACE' ) );
#17162 = CARTESIAN_POINT ( 'NONE',  ( 2.449293598294706513E-15, -20.00000000000000000, -9.000000000000000000 ) ) ;
#17163 = ORIENTED_EDGE ( 'NONE', *, *, #11567, .T. ) ;
#17164 = CARTESIAN_POINT ( 'NONE',  ( -15.51323935927264586, -32.62297130559655045, -9.000000000000000000 ) ) ;
#17165 = DIRECTION ( 'NONE',  ( 0.000000000000000000, 0.000000000000000000, -1.000000000000000000 ) ) ;
#17166 = VERTEX_POINT ( 'NONE', #11261 ) ;
#17167 = AXIS2_PLACEMENT_3D ( 'NONE', #10521, #13570, #142 ) ;
#17168 = AXIS2_PLACEMENT_3D ( 'NONE', #15502, #1795, #705 ) ;
#17169 = FACE_OUTER_BOUND ( 'NONE', #5672, .T. ) ;
#17170 = CARTESIAN_POINT ( 'NONE',  ( -4.175648173966055587, 2.207990556236529844, -3.469390959564062626 ) ) ;
#17171 = CARTESIAN_POINT ( 'NONE',  ( -1.398397006336996817, -6.091550361990593743, 0.000000000000000000 ) ) ;
#17172 = CARTESIAN_POINT ( 'NONE',  ( 1.925929944387235853E-31, 15.00000000000001599, 9.000000000000000000 ) ) ;
#17173 = CARTESIAN_POINT ( 'NONE',  ( -6.473970235329672780E-16, -4.862606272033106691, -3.745885042887442395 ) ) ;
#17174 = CARTESIAN_POINT ( 'NONE',  ( 55.71335778527780747, 46.09948385550240602, 1.832500667257165983 ) ) ;
#17175 = MECHANICAL_DESIGN_GEOMETRIC_PRESENTATION_REPRESENTATION (  '', ( #3103 ), #18443 ) ;
#17176 = CARTESIAN_POINT ( 'NONE',  ( 6.371506350351446635, 5.409331239960136983, 0.8483282427581467777 ) ) ;
#17177 = CARTESIAN_POINT ( 'NONE',  ( 45.90387839640214196, 48.69948385550240744, 5.676469297603166098 ) ) ;
#17178 = CARTESIAN_POINT ( 'NONE',  ( 43.34962307344078880, 62.10051614449766078, -2.184720259617096705 ) ) ;
#17179 = CYLINDRICAL_SURFACE ( 'NONE', #18426, 4.799999999999999822 ) ;
#17180 = DIRECTION ( 'NONE',  ( 0.000000000000000000, -0.4999999999999991118, 0.8660254037844391517 ) ) ;
#17181 = ADVANCED_FACE ( 'NONE', ( #17169 ), #4418, .F. ) ;
#17182 = AXIS2_PLACEMENT_3D ( 'NONE', #18640, #3720, #9684 ) ;
#17183 = CARTESIAN_POINT ( 'NONE',  ( 50.00000000000000000, 74.50000000000002842, 0.000000000000000000 ) ) ;
#17184 = ORIENTED_EDGE ( 'NONE', *, *, #3759, .F. ) ;
#17185 = FACE_OUTER_BOUND ( 'NONE', #18496, .T. ) ;
#17186 = EDGE_CURVE ( 'NONE', #4192, #17315, #12230, .T. ) ;
#17187 = CARTESIAN_POINT ( 'NONE',  ( -0.4472135954999577612, 0.000000000000000000, -4.599999999999999645 ) ) ;
#17188 = CARTESIAN_POINT ( 'NONE',  ( 47.70284917648459810, 53.60051614449766078, 6.992620115222797139 ) ) ;
#17189 = EDGE_CURVE ( 'NONE', #8857, #10940, #11161, .T. ) ;
#17190 = EDGE_CURVE ( 'NONE', #440, #6895, #13910, .T. ) ;
#17191 = CARTESIAN_POINT ( 'NONE',  ( 49.99999999999997158, 45.00000000000001421, -7.499999999999998224 ) ) ;
#17192 = DIRECTION ( 'NONE',  ( -1.000000000000000000, 0.000000000000000000, 0.000000000000000000 ) ) ;
#17193 = ORIENTED_EDGE ( 'NONE', *, *, #5799, .F. ) ;
#17194 = CARTESIAN_POINT ( 'NONE',  ( 0.1085714285714285687, -3.798448662927795372, 0.000000000000000000 ) ) ;
#17195 = DIRECTION ( 'NONE',  ( -0.000000000000000000, -0.000000000000000000, 1.000000000000000000 ) ) ;
#17196 = AXIS2_PLACEMENT_3D ( 'NONE', #18911, #17427, #11332 ) ;
#17197 = EDGE_CURVE ( 'NONE', #15861, #13867, #3784, .T. ) ;
#17198 = LINE ( 'NONE', #7965, #12774 ) ;
#17199 = CARTESIAN_POINT ( 'NONE',  ( 57.36023556966787851, 45.99948385550238328, -0.02388180880522424582 ) ) ;
#17200 = CARTESIAN_POINT ( 'NONE',  ( 5.100000000000002309, 0.000000000000000000, 5.200000000000001066 ) ) ;
#17201 = CARTESIAN_POINT ( 'NONE',  ( 49.97728705011495265, 61.50051614449766646, 8.000000000000001776 ) ) ;
#17202 = CARTESIAN_POINT ( 'NONE',  ( 50.02271294988506156, 62.50051614449767357, -6.000000000000000888 ) ) ;
#17203 = COLOUR_RGB ( '',0.8941176470588234615, 0.8941176470588234615, 0.8941176470588234615 ) ;
#17204 = CARTESIAN_POINT ( 'NONE',  ( 2.449293598294706513E-15, -20.00000000000000000, -9.000000000000000000 ) ) ;
#17205 = CARTESIAN_POINT ( 'NONE',  ( 0.000000000000000000, 0.000000000000000000, -0.8000000000000000444 ) ) ;
#17207 = ORIENTED_EDGE ( 'NONE', *, *, #18997, .F. ) ;
#17206 = EDGE_CURVE ( 'NONE', #16376, #12683, #11278, .T. ) ;
#17208 = EDGE_CURVE ( 'NONE', #71, #1748, #17569, .T. ) ;
#17209 = ORIENTED_EDGE ( 'NONE', *, *, #15675, .F. ) ;
#17210 = VERTEX_POINT ( 'NONE', #5390 ) ;
#17211 = FACE_OUTER_BOUND ( 'NONE', #8028, .T. ) ;
#17212 = ORIENTED_EDGE ( 'NONE', *, *, #2839, .T. ) ;
#17213 = AXIS2_PLACEMENT_3D ( 'NONE', #4253, #1322, #8657 ) ;
#17214 = CARTESIAN_POINT ( 'NONE',  ( 4.033906725095553369, -1.419670120619691334, 3.500000000000000444 ) ) ;
#17215 = EDGE_LOOP ( 'NONE', ( #6559, #1528, #6326, #7516 ) ) ;
#17216 = DIRECTION ( 'NONE',  ( -0.000000000000000000, -0.000000000000000000, 1.000000000000000000 ) ) ;
#17217 = CARTESIAN_POINT ( 'NONE',  ( 45.86712807150323812, 59.29948385550240175, -5.649768623646098220 ) ) ;
#17218 = ORIENTED_EDGE ( 'NONE', *, *, #14844, .T. ) ;
#17219 = CARTESIAN_POINT ( 'NONE',  ( 6.367873360227558344, -2.886751345948133984, -5.000000000000000000 ) ) ;
#17220 = EDGE_LOOP ( 'NONE', ( #9254, #18094, #7747, #129 ) ) ;
#17221 = CARTESIAN_POINT ( 'NONE',  ( 42.38452918213188525, 55.09948385550241312, -2.450534656007040013 ) ) ;
#17222 = CARTESIAN_POINT ( 'NONE',  ( 2.000000000000000000, 1.773042676681340524, -2.059984127722458425E-15 ) ) ;
#17223 = CARTESIAN_POINT ( 'NONE',  ( 52.25172492374522903, 63.59948385550237759, -7.007379884777225953 ) ) ;
#17224 = CARTESIAN_POINT ( 'NONE',  ( 3.961551342853837809, 2.319461885623310682, 2.982574167880912341 ) ) ;
#17225 = CARTESIAN_POINT ( 'NONE',  ( 0.000000000000000000, -0.8865213383406694847, 1.535500000000001419 ) ) ;
#17226 = CARTESIAN_POINT ( 'NONE',  ( 43.34962307344078880, 60.10051614449766078, -2.184720259617096705 ) ) ;
#17227 = AXIS2_PLACEMENT_3D ( 'NONE', #5898, #2877, #17677 ) ;
#17228 = CARTESIAN_POINT ( 'NONE',  ( 44.88205777487398507, 61.19948385550241454, -3.688883143319540814 ) ) ;
#17229 = CARTESIAN_POINT ( 'NONE',  ( 52.25172492374522903, 59.59948385550240602, -7.007379884777225953 ) ) ;
#17230 = CARTESIAN_POINT ( 'NONE',  ( 6.495567275915087535, -2.917443832164882345, 5.053160945538040849 ) ) ;
#17231 = PLANE ( 'NONE',  #8456 ) ;
#17232 = ORIENTED_EDGE ( 'NONE', *, *, #7935, .T. ) ;
#17233 = TOROIDAL_SURFACE ( 'NONE', #10016, 5.899999999999999467, 0.1000000000000010186 ) ;
#17234 = ORIENTED_EDGE ( 'NONE', *, *, #5617, .T. ) ;
#17235 = DIRECTION ( 'NONE',  ( 0.000000000000000000, 0.000000000000000000, -1.000000000000000000 ) ) ;
#17236 = ORIENTED_EDGE ( 'NONE', *, *, #6288, .F. ) ;
#17237 = CARTESIAN_POINT ( 'NONE',  ( 45.86712807150323812, 61.29948385550240886, -5.649768623646098220 ) ) ;
#17238 = ADVANCED_FACE ( 'NONE', ( #12447 ), #5346, .T. ) ;
#17239 = DIRECTION ( 'NONE',  ( -0.000000000000000000, -0.000000000000000000, -1.000000000000000000 ) ) ;
#17240 = ORIENTED_EDGE ( 'NONE', *, *, #8782, .T. ) ;
#17241 = ORIENTED_EDGE ( 'NONE', *, *, #6675, .T. ) ;
#17242 = FACE_OUTER_BOUND ( 'NONE', #10656, .T. ) ;
#17243 = CIRCLE ( 'NONE', #11576, 2.000000000000001776 ) ;
#17244 = B_SPLINE_CURVE_WITH_KNOTS ( 'NONE', 3,
 ( #5877, #13419, #11843, #13704, #4702, #6256 ),
 .UNSPECIFIED., .F., .F.,
 ( 4, 2, 4 ),
 ( -3.640115492409406142E-06, 0.0002066546034006526487, 0.0004169493222937146744 ),
 .UNSPECIFIED. ) ;
#17245 = EDGE_LOOP ( 'NONE', ( #17637, #10344, #1348, #1319 ) ) ;
#17246 = AXIS2_PLACEMENT_3D ( 'NONE', #14800, #3150, #4616 ) ;
#17247 = DIRECTION ( 'NONE',  ( -1.000000000000000000, 0.000000000000000000, 0.000000000000000000 ) ) ;
#17248 = CIRCLE ( 'NONE', #18513, 3.309499999999999886 ) ;
#17249 = EDGE_LOOP ( 'NONE', ( #10083, #15780, #12916, #16177, #18908 ) ) ;
#17250 = CARTESIAN_POINT ( 'NONE',  ( 55.96859303347804371, 48.19948385550240033, 4.306917132069425946 ) ) ;
#17251 = CARTESIAN_POINT ( 'NONE',  ( 4.000000000000000000, 0.9868501483902631932, -0.09357334158579604100 ) ) ;
#17252 = AXIS2_PLACEMENT_3D ( 'NONE', #2790, #2698, #13458 ) ;
#17253 = CARTESIAN_POINT ( 'NONE',  ( 50.02271294988506156, 64.50051614449766646, -6.000000000000000888 ) ) ;
#17254 = LINE ( 'NONE', #3911, #11734 ) ;
#17255 = EDGE_CURVE ( 'NONE', #7505, #7529, #6907, .T. ) ;
#17256 = FACE_BOUND ( 'NONE', #16474, .T. ) ;
#17257 = CARTESIAN_POINT ( 'NONE',  ( 1.925929944387235853E-31, 15.00000000000001599, -9.000000000000000000 ) ) ;
#17258 = AXIS2_PLACEMENT_3D ( 'NONE', #6466, #14202, #17272 ) ;
#17259 = EDGE_CURVE ( 'NONE', #16560, #10123, #19146, .T. ) ;
#17260 = AXIS2_PLACEMENT_3D ( 'NONE', #18322, #16658, #4878 ) ;
#17261 = AXIS2_PLACEMENT_3D ( 'NONE', #831, #8473, #11402 ) ;
#17262 = ORIENTED_EDGE ( 'NONE', *, *, #2095, .F. ) ;
#17263 = ORIENTED_EDGE ( 'NONE', *, *, #5599, .F. ) ;
#17264 = CARTESIAN_POINT ( 'NONE',  ( 4.000000000000000888, -0.8578082829538523635, -3.433262215449808696 ) ) ;
#17265 =( NAMED_UNIT ( * ) PLANE_ANGLE_UNIT ( ) SI_UNIT ( $, .RADIAN. ) );
#17266 = CARTESIAN_POINT ( 'NONE',  ( -62.49999999999997158, 32.50000000000001421, 15.00000000000000000 ) ) ;
#17267 = CARTESIAN_POINT ( 'NONE',  ( 0.000000000000000000, 0.000000000000000000, 0.000000000000000000 ) ) ;
#17268 = ORIENTED_EDGE ( 'NONE', *, *, #17016, .T. ) ;
#17269 = DIRECTION ( 'NONE',  ( 0.000000000000000000, 0.000000000000000000, 1.000000000000000000 ) ) ;
#17270 = CARTESIAN_POINT ( 'NONE',  ( -3.098410542199071749, -7.060458129626440815, 0.000000000000000000 ) ) ;
#17271 = ORIENTED_EDGE ( 'NONE', *, *, #18097, .F. ) ;
#17272 = DIRECTION ( 'NONE',  ( 0.4999999999999974465, 0.8660254037844401509, 0.000000000000000000 ) ) ;
#17273 = CARTESIAN_POINT ( 'NONE',  ( -99.99999999999997158, -6.999999999999989342, -10.00000000000000000 ) ) ;
#17274 = TOROIDAL_SURFACE ( 'NONE', #12878, 5.000000000000000000, 0.5999999999999999778 ) ;
#17275 = CIRCLE ( 'NONE', #1303, 2.649999999999985700 ) ;
#17276 = CARTESIAN_POINT ( 'NONE',  ( 16.79901371501595975, -30.85325472854598416, 9.000000000000000000 ) ) ;
#17277 = DIRECTION ( 'NONE',  ( 0.000000000000000000, 0.000000000000000000, -1.000000000000000000 ) ) ;
#17278 = CARTESIAN_POINT ( 'NONE',  ( 43.69122665457040000, 48.99948385550241170, 0.02388180880521036456 ) ) ;
#17279 = CARTESIAN_POINT ( 'NONE',  ( -4.158233816355195955, -0.4370479853238878887, -9.000000000000000000 ) ) ;
#17280 = CARTESIAN_POINT ( 'NONE',  ( 42.63976443033212860, 48.99948385550240459, 0.02388180880522514787 ) ) ;
#17281 = CARTESIAN_POINT ( 'NONE',  ( 47.74827507625469281, 58.40051614449766504, -7.007379884777203749 ) ) ;
#17282 = CYLINDRICAL_SURFACE ( 'NONE', #6812, 2.149999999999999023 ) ;
#17283 = CARTESIAN_POINT ( 'NONE',  ( 6.242800618755075526, 3.923709308887314950, -3.414402460853798171 ) ) ;
#17284 = APPLICATION_CONTEXT ( 'automotive_design' ) ;
#17285 = DIRECTION ( 'NONE',  ( 6.123233995736766036E-17, 0.000000000000000000, 1.000000000000000000 ) ) ;
#17286 = EDGE_LOOP ( 'NONE', ( #13498, #5358, #13723, #17564, #1143 ) ) ;
#17287 = AXIS2_PLACEMENT_3D ( 'NONE', #11078, #18661, #6473 ) ;
#17288 =( NAMED_UNIT ( * ) SI_UNIT ( $, .STERADIAN. ) SOLID_ANGLE_UNIT ( ) );
#17289 = PRODUCT ( 'motor', 'motor', '', ( #15394 ) ) ;
#17290 = CIRCLE ( 'NONE', #2265, 1.999999999999998224 ) ;
#17291 = CARTESIAN_POINT ( 'NONE',  ( 5.599999999999999645, 0.000000000000000000, 2.500000000000000444 ) ) ;
#17292 = CARTESIAN_POINT ( 'NONE',  ( 56.66441430157294690, 50.90051614449766504, -2.141517661632166281 ) ) ;
#17293 = CARTESIAN_POINT ( 'NONE',  ( 4.104070371397484429, -2.023683613428364669, 3.505122836902509587 ) ) ;
#17294 = DIRECTION ( 'NONE',  ( -1.000000000000000000, 0.000000000000000000, 0.000000000000000000 ) ) ;
#17295 = EDGE_LOOP ( 'NONE', ( #10925, #13032, #3036, #6617 ) ) ;
#17296 = LINE ( 'NONE', #2857, #2431 ) ;
#17297 = FACE_OUTER_BOUND ( 'NONE', #17892, .T. ) ;
#17298 = EDGE_CURVE ( 'NONE', #18807, #3828, #18834, .T. ) ;
#17299 = LINE ( 'NONE', #5412, #11503 ) ;
#17300 = CARTESIAN_POINT ( 'NONE',  ( 55.94051828345050836, 45.79948385550240886, -4.345558710429104465 ) ) ;
#17301 = DIRECTION ( 'NONE',  ( -0.000000000000000000, -0.000000000000000000, 1.000000000000000000 ) ) ;
#17302 = CARTESIAN_POINT ( 'NONE',  ( 41.58830220609386430, 48.99948385550241170, 0.02388180880523263147 ) ) ;
#17303 = DIRECTION ( 'NONE',  ( 0.000000000000000000, 0.000000000000000000, 1.000000000000000000 ) ) ;
#17304 = CARTESIAN_POINT ( 'NONE',  ( 56.30877334542961421, 59.00051614449766646, 0.02388180880515774693 ) ) ;
#17305 = CARTESIAN_POINT ( 'NONE',  ( 0.8816464618332836567, -24.71833652004169934, 9.999999999999998224 ) ) ;
#17306 = DIRECTION ( 'NONE',  ( -1.000000000000000000, 0.000000000000000000, 0.000000000000000000 ) ) ;
#17307 = VERTEX_POINT ( 'NONE', #11361 ) ;
#17308 = VERTEX_POINT ( 'NONE', #11070 ) ;
#17309 = ORIENTED_EDGE ( 'NONE', *, *, #2388, .F. ) ;
#17310 = DIRECTION ( 'NONE',  ( 0.000000000000000000, -0.000000000000000000, 1.000000000000000000 ) ) ;
#17311 = ORIENTED_EDGE ( 'NONE', *, *, #18752, .F. ) ;
#17312 = CARTESIAN_POINT ( 'NONE',  ( 4.158921784487744411, 2.089935040870091409, 3.500000000000000444 ) ) ;
#17313 = EDGE_CURVE ( 'NONE', #6336, #17942, #2471, .T. ) ;
#17314 = CIRCLE ( 'NONE', #401, 4.872650870659752442 ) ;
#17315 = VERTEX_POINT ( 'NONE', #9888 ) ;
#17316 = DIRECTION ( 'NONE',  ( 0.000000000000000000, 0.000000000000000000, -1.000000000000000000 ) ) ;
#17317 = CARTESIAN_POINT ( 'NONE',  ( 50.02271294988512551, 58.49948385550241170, 7.000000000000000888 ) ) ;
#17318 = EDGE_LOOP ( 'NONE', ( #18033, #8564, #18246, #12518 ) ) ;
#17319 = LINE ( 'NONE', #3971, #6182 ) ;
#17320 = ORIENTED_EDGE ( 'NONE', *, *, #3699, .T. ) ;
#17321 = CARTESIAN_POINT ( 'NONE',  ( 47.37792948025162332, 55.39948385550240317, -7.992620115222770494 ) ) ;
#17322 = CARTESIAN_POINT ( 'NONE',  ( -154.9999999999999716, -14.99999999999999645, 17.00000000000000000 ) ) ;
#17323 = ADVANCED_FACE ( 'NONE', ( #8529 ), #4120, .T. ) ;
#17324 = CARTESIAN_POINT ( 'NONE',  ( 48.07319477248768180, 52.59948385550240602, 6.007379884777225953 ) ) ;
#17325 = DIRECTION ( 'NONE',  ( -1.000000000000000000, 0.000000000000000000, 0.000000000000000000 ) ) ;
#17326 = EDGE_CURVE ( 'NONE', #2828, #17434, #1082, .T. ) ;
#17327 = DIRECTION ( 'NONE',  ( 0.000000000000000000, 0.000000000000000000, -1.000000000000000000 ) ) ;
#17328 = CARTESIAN_POINT ( 'NONE',  ( 52.57664461997821093, 45.40051614449765793, 8.007379884777206414 ) ) ;
#17329 = CARTESIAN_POINT ( 'NONE',  ( 46.45491332379572924, 61.29948385550240886, -4.840751629271157874 ) ) ;
#17330 = CARTESIAN_POINT ( 'NONE',  ( 45.15499999999999403, 3.061616997868383634E-16, -2.500000000000000444 ) ) ;
#17331 = DIRECTION ( 'NONE',  ( 0.000000000000000000, -0.000000000000000000, 1.000000000000000000 ) ) ;
#17332 = ORIENTED_EDGE ( 'NONE', *, *, #4748, .F. ) ;
#17333 = EDGE_CURVE ( 'NONE', #16171, #666, #1913, .T. ) ;
#17334 = ADVANCED_FACE ( 'NONE', ( #18943 ), #8819, .T. ) ;
#17335 = CARTESIAN_POINT ( 'NONE',  ( 56.66441430157296821, 60.09948385550240602, 2.141517661632100111 ) ) ;
#17336 =( BOUNDED_SURFACE ( )  B_SPLINE_SURFACE ( 3, 2, ( 
 ( #9446, #3202, #9164 ),
 ( #1918, #10910, #7785 ),
 ( #18393, #7885, #6224 ),
 ( #15142, #13944, #15235 ),
 ( #18297, #7687, #9535 ),
 ( #527, #1719, #624 ) ),
 .UNSPECIFIED., .F., .F., .T. ) 
 B_SPLINE_SURFACE_WITH_KNOTS ( ( 4, 2, 4 ),
 ( 3, 3 ),
 ( 0.02367865728600892020, 0.02663179453327098323, 0.02958493178053304279 ),
 ( 0.000000000000000000, 1.000000000000000000 ),
 .UNSPECIFIED. ) 
 GEOMETRIC_REPRESENTATION_ITEM ( )  RATIONAL_B_SPLINE_SURFACE ( (
 ( 1.000000000000000000, 0.8047781103519402457, 1.000000000000000000),
 ( 1.000000000000000000, 0.8123785825973208752, 1.000000000000000000),
 ( 1.000000000000000000, 0.8190671539297160741, 1.000000000000000000),
 ( 1.000000000000000000, 0.8192352255325974220, 1.000000000000000000),
 ( 1.000000000000000000, 0.8126129676842754890, 1.000000000000000000),
 ( 1.000000000000000000, 0.8047712537969723412, 1.000000000000000000) ) ) 
 REPRESENTATION_ITEM ( '' )  SURFACE ( )  );
#17337 = ORIENTED_EDGE ( 'NONE', *, *, #2329, .F. ) ;
#17338 = DIRECTION ( 'NONE',  ( 1.000000000000000000, 0.000000000000000000, 0.000000000000000000 ) ) ;
#17339 = FILL_AREA_STYLE ('',( #2336 ) ) ;
#17340 = VERTEX_POINT ( 'NONE', #15887 ) ;
#17341 = EDGE_CURVE ( 'NONE', #7385, #12254, #7532, .T. ) ;
#17342 = CARTESIAN_POINT ( 'NONE',  ( 52.29715082351547295, 58.39948385550238896, 6.992620115222774047 ) ) ;
#17343 = DIRECTION ( 'NONE',  ( -1.000000000000000000, -0.000000000000000000, -0.000000000000000000 ) ) ;
#17344 = ORIENTED_EDGE ( 'NONE', *, *, #10524, .T. ) ;
#17345 = EDGE_LOOP ( 'NONE', ( #3237, #11177, #1172, #3875 ) ) ;
#17346 = CARTESIAN_POINT ( 'NONE',  ( 0.1481481481481481122, -4.797713218419819903, -1.000000000000000000 ) ) ;
#17347 = ORIENTED_EDGE ( 'NONE', *, *, #6851, .T. ) ;
#17348 = ORIENTED_EDGE ( 'NONE', *, *, #18452, .T. ) ;
#17349 = CARTESIAN_POINT ( 'NONE',  ( 52.25172492374522903, 53.59948385550241312, -7.007379884777225953 ) ) ;
#17350 = FACE_OUTER_BOUND ( 'NONE', #7725, .T. ) ;
#17351 = CARTESIAN_POINT ( 'NONE',  ( 51.97223112728249816, 58.60051614449766788, -5.992620115222793586 ) ) ;
#17352 = DIRECTION ( 'NONE',  ( 0.000000000000000000, 0.000000000000000000, -1.000000000000000000 ) ) ;
#17353 = CARTESIAN_POINT ( 'NONE',  ( 14.00000000000000000, 1.610000000000000098, 0.000000000000000000 ) ) ;
#17354 = PLANE ( 'NONE',  #962 ) ;
#17355 = CONICAL_SURFACE ( 'NONE', #1070, 4.000000000000003553, 1.029744260000001077 ) ;
#17356 = ORIENTED_EDGE ( 'NONE', *, *, #6261, .T. ) ;
#17357 = VERTEX_POINT ( 'NONE', #4212 ) ;
#17358 = CARTESIAN_POINT ( 'NONE',  ( 4.000000000001088907, 1.658577278524410170, -3.531553309554541720 ) ) ;
#17359 = CARTESIAN_POINT ( 'NONE',  ( 1.000000000000000000, -6.008326913195983998, 0.000000000000000000 ) ) ;
#17360 = CARTESIAN_POINT ( 'NONE',  ( 2.449293598294706513E-15, -20.00000000000000000, 9.000000000000000000 ) ) ;
#17361 = CONTEXT_DEPENDENT_SHAPE_REPRESENTATION ( #15678, #18864 ) ;
#17362 = ORIENTED_EDGE ( 'NONE', *, *, #6804, .F. ) ;
#17363 = CARTESIAN_POINT ( 'NONE',  ( 6.092449800118089343, 4.833012432206481357, 1.628976913806340798 ) ) ;
#17364 = EDGE_CURVE ( 'NONE', #13076, #4248, #8480, .T. ) ;
#17365 = ORIENTED_EDGE ( 'NONE', *, *, #1854, .T. ) ;
#17366 = EDGE_CURVE ( 'NONE', #2192, #13670, #9985, .T. ) ;
#17367 = AXIS2_PLACEMENT_3D ( 'NONE', #9435, #11188, #7963 ) ;
#17368 = DIRECTION ( 'NONE',  ( 0.000000000000000000, 0.000000000000000000, 1.000000000000000000 ) ) ;
#17369 = CARTESIAN_POINT ( 'NONE',  ( 5.686050877451574337, -5.768780236673276995, -1.000000000000000000 ) ) ;
#17370 = CIRCLE ( 'NONE', #7336, 14.00000000000000000 ) ;
#17371 = CARTESIAN_POINT ( 'NONE',  ( 48.02776887271745210, 63.39948385550238896, -5.992620115222778487 ) ) ;
#17372 = CARTESIAN_POINT ( 'NONE',  ( 2.449293598294706513E-15, -20.00000000000000000, -20.00000000000000000 ) ) ;
#17373 = DIRECTION ( 'NONE',  ( 1.000000000000000000, 0.000000000000000000, 0.000000000000000000 ) ) ;
#17374 = CARTESIAN_POINT ( 'NONE',  ( 55.11794222512601493, 52.19948385550240744, 3.688883143319541702 ) ) ;
#17375 = DIRECTION ( 'NONE',  ( -0.7071067811865530128, 8.659560562354868763E-17, -0.7071067811865421326 ) ) ;
#17376 = CARTESIAN_POINT ( 'NONE',  ( 43.34962307344081012, 46.89948385550240317, 2.184720259617164650 ) ) ;
#17377 = CARTESIAN_POINT ( 'NONE',  ( 56.79116909180259398, 47.20051614449766220, 4.963592699178938972 ) ) ;
#17378 = CARTESIAN_POINT ( 'NONE',  ( 8.500000000000000000, 0.000000000000000000, 0.000000000000000000 ) ) ;
#17379 = FACE_OUTER_BOUND ( 'NONE', #12855, .T. ) ;
#17380 = DIRECTION ( 'NONE',  ( 1.000000000000000000, 0.000000000000000000, 0.000000000000000000 ) ) ;
#17381 = EDGE_LOOP ( 'NONE', ( #8212, #18083, #12548, #1872 ) ) ;
#17382 = AXIS2_PLACEMENT_3D ( 'NONE', #14994, #17960, #4314 ) ;
#17383 = CYLINDRICAL_SURFACE ( 'NONE', #17386, 4.000000000000003553 ) ;
#17384 = CARTESIAN_POINT ( 'NONE',  ( 1.171083334267915221, -24.65495046420793201, 9.999999999999998224 ) ) ;
#17385 = CARTESIAN_POINT ( 'NONE',  ( 42.63976443033212149, 54.00051614449765935, -0.02388180880514948964 ) ) ;
#17386 = AXIS2_PLACEMENT_3D ( 'NONE', #9170, #15710, #9608 ) ;
#17387 = CARTESIAN_POINT ( 'NONE',  ( -74.99999999999998579, -7.500000000000027534, -10.00000000000000000 ) ) ;
#17388 = CARTESIAN_POINT ( 'NONE',  ( -20.63749999999999574, 0.000000000000000000, 0.000000000000000000 ) ) ;
#17389 = ADVANCED_BREP_SHAPE_REPRESENTATION ( '', ( #8977, #10359 ), #4043 ) ;
#17390 = EDGE_LOOP ( 'NONE', ( #6078, #8205, #10653, #1927 ) ) ;
#17391 = LINE ( 'NONE', #5783, #3657 ) ;
#17392 = DIRECTION ( 'NONE',  ( -1.000000000000000000, 0.000000000000000000, 0.000000000000000000 ) ) ;
#17393 = FACE_OUTER_BOUND ( 'NONE', #10078, .T. ) ;
#17394 = CARTESIAN_POINT ( 'NONE',  ( 54.09612160359786515, 51.69948385550240744, -5.676469297603166098 ) ) ;
#17395 = CIRCLE ( 'NONE', #1418, 24.99999999999999289 ) ;
#17396 = FACE_OUTER_BOUND ( 'NONE', #7394, .T. ) ;
#17397 = CARTESIAN_POINT ( 'NONE',  ( 42.38452918213188525, 49.09948385550241312, -2.450534656007040013 ) ) ;
#17398 = CIRCLE ( 'NONE', #12650, 0.9999999999999995559 ) ;
#17399 = DIRECTION ( 'NONE',  ( -0.000000000000000000, -0.000000000000000000, 1.000000000000000000 ) ) ;
#17400 = CARTESIAN_POINT ( 'NONE',  ( 45.86712807150329496, 47.70051614449766220, 5.649768623646139964 ) ) ;
#17401 = CARTESIAN_POINT ( 'NONE',  ( -1.000000000000000000, -14.00000000000000000, 8.999999999999998224 ) ) ;
#17402 = FACE_OUTER_BOUND ( 'NONE', #18111, .T. ) ;
#17403 = ORIENTED_EDGE ( 'NONE', *, *, #12431, .F. ) ;
#17404 = ORIENTED_EDGE ( 'NONE', *, *, #10577, .F. ) ;
#17405 = PLANE ( 'NONE',  #1552 ) ;
#17406 = EDGE_LOOP ( 'NONE', ( #18978, #7623, #8265, #13975 ) ) ;
#17407 = DIRECTION ( 'NONE',  ( 0.000000000000000000, 1.000000000000000000, 0.000000000000000000 ) ) ;
#17408 = ORIENTED_EDGE ( 'NONE', *, *, #281, .F. ) ;
#17409 = CARTESIAN_POINT ( 'NONE',  ( 6.367873360227556567, 2.886751345948123770, -5.000000000000000000 ) ) ;
#17410 = CARTESIAN_POINT ( 'NONE',  ( 45.90387839640214196, 56.69948385550240744, 5.676469297603166098 ) ) ;
#17411 = VERTEX_POINT ( 'NONE', #2760 ) ;
#17412 = LINE ( 'NONE', #9934, #7724 ) ;
#17413 = ORIENTED_EDGE ( 'NONE', *, *, #8072, .T. ) ;
#17414 = CARTESIAN_POINT ( 'NONE',  ( 42.39856655714566358, 58.89948385550241028, 2.493737253992119207 ) ) ;
#17415 = CARTESIAN_POINT ( 'NONE',  ( 0.3126073911696399255, 2.020725942163686284, -3.499999999999999556 ) ) ;
#17416 = VECTOR ( 'NONE', #17560, 1000.000000000000114 ) ;
#17417 = CARTESIAN_POINT ( 'NONE',  ( 44.30067958973596376, 52.89948385550241028, 1.875703265242204099 ) ) ;
#17418 = CARTESIAN_POINT ( 'NONE',  ( 2.595115354961440524, -7.673029147243177306, 0.000000000000000000 ) ) ;
#17419 = CARTESIAN_POINT ( 'NONE',  ( 1.150000000000001688, 0.000000000000000000, -6.000000000000000888 ) ) ;
#17420 = CARTESIAN_POINT ( 'NONE',  ( 57.61547081786810764, 48.90051614449766504, -2.450534656007114176 ) ) ;
#17421 = CARTESIAN_POINT ( 'NONE',  ( 44.30067958973596376, 64.89948385550239607, 1.875703265242204099 ) ) ;
#17422 = CIRCLE ( 'NONE', #500, 4.872650870659752442 ) ;
#17423 = CARTESIAN_POINT ( 'NONE',  ( 6.481779955677443361, -2.910222513313286186, 5.040653254389420468 ) ) ;
#17424 = LINE ( 'NONE', #9760, #15656 ) ;
#17425 = ORIENTED_EDGE ( 'NONE', *, *, #8309, .T. ) ;
#17426 = ORIENTED_EDGE ( 'NONE', *, *, #15767, .F. ) ;
#17427 = DIRECTION ( 'NONE',  ( 0.000000000000000000, 0.000000000000000000, -1.000000000000000000 ) ) ;
#17428 = APPLICATION_PROTOCOL_DEFINITION ( 'draft international standard', 'automotive_design', 1998, #10873 ) ;
#17429 = ORIENTED_EDGE ( 'NONE', *, *, #15205, .T. ) ;
#17430 = ADVANCED_FACE ( 'NONE', ( #7344 ), #13320, .F. ) ;
#17431 = CARTESIAN_POINT ( 'NONE',  ( 54.09612160359786515, 57.69948385550240744, -5.676469297603166098 ) ) ;
#17432 = CYLINDRICAL_SURFACE ( 'NONE', #18768, 2.000000000000001776 ) ;
#17433 =( REPRESENTATION_RELATIONSHIP ('NONE','NONE', #16703, #9916 ) REPRESENTATION_RELATIONSHIP_WITH_TRANSFORMATION ( #4626 )SHAPE_REPRESENTATION_RELATIONSHIP( ) );
#17434 = VERTEX_POINT ( 'NONE', #14593 ) ;
#17435 = ORIENTED_EDGE ( 'NONE', *, *, #9632, .F. ) ;
#17436 = CARTESIAN_POINT ( 'NONE',  ( -1.000000000000000000, -5.408326913195983465, 0.000000000000000000 ) ) ;
#17437 = EDGE_CURVE ( 'NONE', #19163, #8753, #7545, .T. ) ;
#17438 = ORIENTED_EDGE ( 'NONE', *, *, #11309, .T. ) ;
#17439 = DIRECTION ( 'NONE',  ( 0.000000000000000000, 0.000000000000000000, -1.000000000000000000 ) ) ;
#17440 = EDGE_LOOP ( 'NONE', ( #6283, #13358, #1710, #8393 ) ) ;
#17441 = EDGE_CURVE ( 'NONE', #3771, #15125, #5654, .T. ) ;
#17442 = ADVANCED_FACE ( 'NONE', ( #17752 ), #8718, .T. ) ;
#17443 = CARTESIAN_POINT ( 'NONE',  ( 49.97728705011488159, 49.49948385550240459, -7.000000000000000888 ) ) ;
#17444 = CARTESIAN_POINT ( 'NONE',  ( 4.000000000000000000, 0.1981133338132474442, 2.382280164152719704E-17 ) ) ;
#17445 = VECTOR ( 'NONE', #5932, 1000.000000000000000 ) ;
#17446 = CARTESIAN_POINT ( 'NONE',  ( 55.96859303347802239, 46.80051614449767072, -4.306917132069484566 ) ) ;
#17447 = DIRECTION ( 'NONE',  ( -0.000000000000000000, -0.000000000000000000, -1.000000000000000000 ) ) ;
#17448 =( NAMED_UNIT ( * ) PLANE_ANGLE_UNIT ( ) SI_UNIT ( $, .RADIAN. ) );
#17449 = CARTESIAN_POINT ( 'NONE',  ( 16.79901371501573593, -9.146745271453662340, 9.000000000000000000 ) ) ;
#17450 = SHAPE_REPRESENTATION ( 'hex flange nut gradea_iso_ISO - 4161 - M5 - N', ( #10359 ), #11543 ) ;
#17451 = ORIENTED_EDGE ( 'NONE', *, *, #6870, .T. ) ;
#17452 = ORIENTED_EDGE ( 'NONE', *, *, #10519, .T. ) ;
#17453 = CARTESIAN_POINT ( 'NONE',  ( 3.020236159542449172, -23.98474259401938014, -9.999999999999994671 ) ) ;
#17454 = EDGE_CURVE ( 'NONE', #5652, #11251, #3478, .T. ) ;
#17455 = AXIS2_PLACEMENT_3D ( 'NONE', #16906, #18580, #6485 ) ;
#17456 = DIRECTION ( 'NONE',  ( 0.000000000000000000, 0.000000000000000000, -1.000000000000000000 ) ) ;
#17457 = EDGE_CURVE ( 'NONE', #11891, #5733, #13034, .T. ) ;
#17458 = DIRECTION ( 'NONE',  ( 0.000000000000000000, 1.224646799147353207E-16, 1.000000000000000000 ) ) ;
#17459 = VERTEX_POINT ( 'NONE', #6957 ) ;
#17460 = CIRCLE ( 'NONE', #7427, 4.800000000000000711 ) ;
#17461 = CARTESIAN_POINT ( 'NONE',  ( -54.99999999999996447, -6.999999999999985789, 10.00000000000000000 ) ) ;
#17462 = ORIENTED_EDGE ( 'NONE', *, *, #18278, .F. ) ;
#17463 = ORIENTED_EDGE ( 'NONE', *, *, #4249, .T. ) ;
#17464 = CARTESIAN_POINT ( 'NONE',  ( 16.79901371501573593, -9.146745271453662340, 0.000000000000000000 ) ) ;
#17465 = CARTESIAN_POINT ( 'NONE',  ( 0.000000000000000000, 0.000000000000000000, -3.499999999999999556 ) ) ;
#17466 = AXIS2_PLACEMENT_3D ( 'NONE', #9031, #11771, #5903 ) ;
#17467 = CARTESIAN_POINT ( 'NONE',  ( 56.30877334542961421, 51.00051614449765935, 0.02388180880515774693 ) ) ;
#17468 = CARTESIAN_POINT ( 'NONE',  ( -2.321707774797442170, -4.824281976789052351, 0.000000000000000000 ) ) ;
#17469 = AXIS2_PLACEMENT_3D ( 'NONE', #11867, #5804, #5900 ) ;
#17470 = DIRECTION ( 'NONE',  ( -1.000000000000000000, -0.000000000000000000, -0.000000000000000000 ) ) ;
#17471 = CARTESIAN_POINT ( 'NONE',  ( 55.71335778527780747, 50.09948385550240602, 1.832500667257165983 ) ) ;
#17472 = DIRECTION ( 'NONE',  ( 0.000000000000000000, 0.000000000000000000, 1.000000000000000000 ) ) ;
#17473 = VECTOR ( 'NONE', #15747, 1000.000000000000114 ) ;
#17474 = CARTESIAN_POINT ( 'NONE',  ( 52.29715082351547295, 46.39948385550240317, 6.992620115222774047 ) ) ;
#17475 = CARTESIAN_POINT ( 'NONE',  ( 56.79116909180259398, 45.20051614449766220, 4.963592699178938972 ) ) ;
#17476 = CARTESIAN_POINT ( 'NONE',  ( 4.093692494532771953, -2.021783646005774759, -3.501831996793842716 ) ) ;
#17477 = CARTESIAN_POINT ( 'NONE',  ( 62.49999999999998579, 40.00000000000001421, 0.000000000000000000 ) ) ;
#17478 = CARTESIAN_POINT ( 'NONE',  ( -44.99999999999997158, -7.499999999999971578, -20.00000000000000000 ) ) ;
#17479 = ADVANCED_FACE ( 'NONE', ( #11847 ), #16281, .F. ) ;
#17480 = ORIENTED_EDGE ( 'NONE', *, *, #1495, .T. ) ;
#17481 = CARTESIAN_POINT ( 'NONE',  ( -0.6810597143197697489, -4.461075778259609770, -3.598441714920717516 ) ) ;
#17482 = CIRCLE ( 'NONE', #15590, 15.00000000000000000 ) ;
#17483 = EDGE_CURVE ( 'NONE', #2940, #5141, #18507, .T. ) ;
#17484 = DIRECTION ( 'NONE',  ( -1.000000000000000000, 0.000000000000000000, 0.000000000000000000 ) ) ;
#17485 = CARTESIAN_POINT ( 'NONE',  ( 55.94051828345054389, 53.20051614449766220, 4.345558710429044957 ) ) ;
#17486 = CARTESIAN_POINT ( 'NONE',  ( 6.534838248920900483, -5.903531555104836848, 4.671345613696493211E-16 ) ) ;
#17487 = FACE_OUTER_BOUND ( 'NONE', #8859, .T. ) ;
#17488 = ORIENTED_EDGE ( 'NONE', *, *, #934, .T. ) ;
#17489 = FACE_OUTER_BOUND ( 'NONE', #2308, .T. ) ;
#17490 = DIRECTION ( 'NONE',  ( 0.000000000000000000, 0.000000000000000000, 1.000000000000000000 ) ) ;
#17491 = CARTESIAN_POINT ( 'NONE',  ( 52.29715082351547295, 52.39948385550241738, 6.992620115222774047 ) ) ;
#17492 = DIRECTION ( 'NONE',  ( -1.000000000000000000, 0.000000000000000000, 0.000000000000000000 ) ) ;
#17493 = CARTESIAN_POINT ( 'NONE',  ( 49.97728705011486738, 45.49948385550240459, -8.000000000000001776 ) ) ;
#17494 = CONICAL_SURFACE ( 'NONE', #9640, 4.000000000000000000, 0.8911886515913786111 ) ;
#17495 = CARTESIAN_POINT ( 'NONE',  ( 42.63976443033212860, 48.00051614449766646, -0.02388180880514948964 ) ) ;
#17496 = EDGE_CURVE ( 'NONE', #17308, #6185, #13614, .T. ) ;
#17497 = AXIS2_PLACEMENT_3D ( 'NONE', #16776, #7840, #13023 ) ;
#17498 = DIRECTION ( 'NONE',  ( 0.000000000000000000, 0.000000000000000000, -1.000000000000000000 ) ) ;
#17499 = CARTESIAN_POINT ( 'NONE',  ( -20.00000000000000000, -19.99999999999999289, -20.00000000000000000 ) ) ;
#17500 = ORIENTED_EDGE ( 'NONE', *, *, #5669, .F. ) ;
#17501 = EDGE_CURVE ( 'NONE', #15433, #4109, #12140, .T. ) ;
#17502 = ORIENTED_EDGE ( 'NONE', *, *, #17075, .F. ) ;
#17503 = DIRECTION ( 'NONE',  ( 0.6040472319084893016, -0.7969485188038759604, -1.107688701425240097E-17 ) ) ;
#17504 = ORIENTED_EDGE ( 'NONE', *, *, #2978, .F. ) ;
#17505 = CARTESIAN_POINT ( 'NONE',  ( -4.000000000000000888, 1.563622288139195238, -0.2253451193528307472 ) ) ;
#17506 = ORIENTED_EDGE ( 'NONE', *, *, #8931, .F. ) ;
#17507 = CARTESIAN_POINT ( 'NONE',  ( 4.154306624731137099, 2.398490048084935822, -3.721999068284414847 ) ) ;
#17508 = AXIS2_PLACEMENT_3D ( 'NONE', #1244, #5949, #3011 ) ;
#17509 = CARTESIAN_POINT ( 'NONE',  ( 55.96859303347805081, 60.19948385550240033, 4.306917132069425058 ) ) ;
#17510 = TOROIDAL_SURFACE ( 'NONE', #15933, 5.000000000000000000, 0.5999999999999999778 ) ;
#17511 = VERTEX_POINT ( 'NONE', #193 ) ;
#17512 = CARTESIAN_POINT ( 'NONE',  ( -6.080745460913608902, 0.5192545390863924082, 0.000000000000000000 ) ) ;
#17513 = ORIENTED_EDGE ( 'NONE', *, *, #19377, .F. ) ;
#17514 = CARTESIAN_POINT ( 'NONE',  ( 49.97728705011486738, 61.49948385550241170, -8.000000000000001776 ) ) ;
#17515 = CARTESIAN_POINT ( 'NONE',  ( 2.449293598294706513E-15, -20.00000000000000000, 9.000000000000000000 ) ) ;
#17516 = CARTESIAN_POINT ( 'NONE',  ( 53.50833635130540955, 49.69948385550240744, -4.867452303228209765 ) ) ;
#17517 = CARTESIAN_POINT ( 'NONE',  ( 0.000000000000000000, 0.000000000000000000, 0.000000000000000000 ) ) ;
#17518 = DIRECTION ( 'NONE',  ( -0.000000000000000000, 0.8660254037844383745, 0.5000000000000004441 ) ) ;
#17519 = MECHANICAL_DESIGN_GEOMETRIC_PRESENTATION_REPRESENTATION (  '', ( #6534 ), #5278 ) ;
#17520 = CARTESIAN_POINT ( 'NONE',  ( 50.02271294988505446, 64.50051614449765225, -7.000000000000000888 ) ) ;
#17521 = CARTESIAN_POINT ( 'NONE',  ( 46.45491332379576477, 49.70051614449766220, 4.840751629271188961 ) ) ;
#17522 = CARTESIAN_POINT ( 'NONE',  ( 45.60000000000000142, 0.000000000000000000, 0.000000000000000000 ) ) ;
#17523 = DIRECTION ( 'NONE',  ( 0.000000000000000000, 0.000000000000000000, -1.000000000000000000 ) ) ;
#17524 = ORIENTED_EDGE ( 'NONE', *, *, #18992, .F. ) ;
#17525 = VECTOR ( 'NONE', #16149, 1000.000000000000000 ) ;
#17526 = ORIENTED_EDGE ( 'NONE', *, *, #15847, .F. ) ;
#17527 = CARTESIAN_POINT ( 'NONE',  ( 0.1217565302851095904, 2.351289329882149559, 2.927447417349536618 ) ) ;
#17528 = PRODUCT_CONTEXT ( 'NONE', #11246, 'mechanical' ) ;
#17529 = ORIENTED_EDGE ( 'NONE', *, *, #15162, .T. ) ;
#17530 = CARTESIAN_POINT ( 'NONE',  ( 44.05948171654949874, 60.79948385550240886, 4.345558710429105354 ) ) ;
#17531 = SURFACE_STYLE_USAGE ( .BOTH. , #11523 ) ;
#17532 = PRESENTATION_LAYER_ASSIGNMENT (  '', '', ( #18154 ) ) ;
#17533 = EDGE_LOOP ( 'NONE', ( #8006, #4558, #18716, #2256 ) ) ;
#17534 = ORIENTED_EDGE ( 'NONE', *, *, #14633, .T. ) ;
#17535 = CYLINDRICAL_SURFACE ( 'NONE', #19326, 24.99999999999999289 ) ;
#17536 = ORIENTED_EDGE ( 'NONE', *, *, #11061, .F. ) ;
#17537 = CARTESIAN_POINT ( 'NONE',  ( 0.3106000600989293203, 5.537975084925940372, 0.4079457818577097994 ) ) ;
#17538 = VERTEX_POINT ( 'NONE', #4707 ) ;
#17539 = AXIS2_PLACEMENT_3D ( 'NONE', #901, #18667, #8245 ) ;
#17540 = CARTESIAN_POINT ( 'NONE',  ( -0.6640947660597427138, 4.471078309994878985, -3.602146406945963442 ) ) ;
#17541 = CARTESIAN_POINT ( 'NONE',  ( 52.29715082351547295, 50.39948385550240317, 6.992620115222774047 ) ) ;
#17542 = CYLINDRICAL_SURFACE ( 'NONE', #19036, 2.500000000000000444 ) ;
#17543 = CARTESIAN_POINT ( 'NONE',  ( 55.96859303347802239, 50.80051614449766362, -4.306917132069484566 ) ) ;
#17544 = CARTESIAN_POINT ( 'NONE',  ( -154.9999999999999716, -6.999999999999993783, -10.00000000000000000 ) ) ;
#17545 = EDGE_CURVE ( 'NONE', #1202, #2689, #18170, .T. ) ;
#17546 = DIRECTION ( 'NONE',  ( 0.000000000000000000, 0.000000000000000000, 1.000000000000000000 ) ) ;
#17547 = AXIS2_PLACEMENT_3D ( 'NONE', #3597, #2129, #2239 ) ;
#17548 = DIRECTION ( 'NONE',  ( 0.000000000000000000, 0.000000000000000000, 1.000000000000000000 ) ) ;
#17549 = ADVANCED_FACE ( 'NONE', ( #13425 ), #7541, .F. ) ;
#17550 = ORIENTED_EDGE ( 'NONE', *, *, #16280, .T. ) ;
#17551 = ORIENTED_EDGE ( 'NONE', *, *, #11956, .F. ) ;
#17552 = FACE_OUTER_BOUND ( 'NONE', #11554, .T. ) ;
#17553 = CONICAL_SURFACE ( 'NONE', #2205, 5.560781378645573980, 1.221730476396046816 ) ;
#17554 = ADVANCED_FACE ( 'NONE', ( #12048 ), #16572, .F. ) ;
#17555 = ADVANCED_FACE ( 'NONE', ( #3144 ), #4726, .T. ) ;
#17556 = FACE_OUTER_BOUND ( 'NONE', #4967, .T. ) ;
#17557 = FILL_AREA_STYLE_COLOUR ( '', #5274 ) ;
#17558 = AXIS2_PLACEMENT_3D ( 'NONE', #16826, #15345, #1928 ) ;
#17559 = ORIENTED_EDGE ( 'NONE', *, *, #7288, .T. ) ;
#17560 = DIRECTION ( 'NONE',  ( 0.000000000000000000, -0.5000000000000011102, -0.8660254037844379305 ) ) ;
#17561 = EDGE_CURVE ( 'NONE', #4790, #7410, #18616, .T. ) ;
#17562 = EDGE_CURVE ( 'NONE', #6796, #7366, #3329, .T. ) ;
#17563 = VECTOR ( 'NONE', #2306, 1000.000000000000000 ) ;
#17564 = ORIENTED_EDGE ( 'NONE', *, *, #19255, .T. ) ;
#17565 = EDGE_LOOP ( 'NONE', ( #13691, #2988, #8442, #16123 ) ) ;
#17566 = CARTESIAN_POINT ( 'NONE',  ( 0.000000000000000000, 0.000000000000000000, -1.000000000000000000 ) ) ;
#17567 = DIRECTION ( 'NONE',  ( 0.000000000000000000, 0.000000000000000000, -1.000000000000000000 ) ) ;
#17569 = CIRCLE ( 'NONE', #14729, 2.100000000000000089 ) ;
#17568 = CARTESIAN_POINT ( 'NONE',  ( 44.28664221472221385, 51.90051614449765793, 1.832500667257213722 ) ) ;
#17570 = CYLINDRICAL_SURFACE ( 'NONE', #10475, 20.00000000000000000 ) ;
#17571 = EDGE_CURVE ( 'NONE', #1014, #7410, #18204, .T. ) ;
#17572 = CARTESIAN_POINT ( 'NONE',  ( 4.175572532730931208, 2.061029303918050726, 3.569807470274392713 ) ) ;
#17573 = EDGE_CURVE ( 'NONE', #16533, #15771, #12241, .T. ) ;
#17574 = CARTESIAN_POINT ( 'NONE',  ( 55.08986747509847248, 53.79948385550241596, -3.727524721679197572 ) ) ;
#17575 = AXIS2_PLACEMENT_3D ( 'NONE', #16969, #3337, #7925 ) ;
#17576 = DIRECTION ( 'NONE',  ( 1.000000000000000000, 0.000000000000000000, 0.000000000000000000 ) ) ;
#17577 = AXIS2_PLACEMENT_3D ( 'NONE', #7580, #17898, #13269 ) ;
#17578 = CARTESIAN_POINT ( 'NONE',  ( 47.74827507625478518, 48.59948385550239180, 7.007379884777227730 ) ) ;
#17579 = CARTESIAN_POINT ( 'NONE',  ( 49.97728705011495265, 47.50051614449765935, 8.000000000000001776 ) ) ;
#17580 = FACE_OUTER_BOUND ( 'NONE', #11516, .T. ) ;
#17581 = AXIS2_PLACEMENT_3D ( 'NONE', #2286, #3940, #8239 ) ;
#17582 = CYLINDRICAL_SURFACE ( 'NONE', #5260, 1.000000000000000000 ) ;
#17583 = EDGE_CURVE ( 'NONE', #8297, #13080, #12550, .T. ) ;
#17584 = DIRECTION ( 'NONE',  ( 1.000000000000000000, 0.000000000000000000, 0.000000000000000000 ) ) ;
#17585 = ORIENTED_EDGE ( 'NONE', *, *, #12167, .T. ) ;
#17586 = VECTOR ( 'NONE', #17955, 1000.000000000000000 ) ;
#17587 = DIRECTION ( 'NONE',  ( 0.000000000000000000, 0.000000000000000000, 1.000000000000000000 ) ) ;
#17588 = CYLINDRICAL_SURFACE ( 'NONE', #9378, 20.00000000000000000 ) ;
#17589 = VECTOR ( 'NONE', #6539, 1000.000000000000000 ) ;
#17590 = VECTOR ( 'NONE', #17498, 1000.000000000000000 ) ;
#17591 = CARTESIAN_POINT ( 'NONE',  ( 43.33558569842706021, 53.90051614449765793, 2.141517661632167169 ) ) ;
#17592 = CARTESIAN_POINT ( 'NONE',  ( 2.321707774797442170, -4.824281976789052351, 0.000000000000000000 ) ) ;
#17593 = FACE_OUTER_BOUND ( 'NONE', #5756, .T. ) ;
#17594 = EDGE_LOOP ( 'NONE', ( #9210, #14373, #1079, #8210 ) ) ;
#17595 = FACE_OUTER_BOUND ( 'NONE', #12308, .T. ) ;
#17596 = CARTESIAN_POINT ( 'NONE',  ( 7.336184427528458230, 0.000000000000000000, -8.105212085995399107 ) ) ;
#17597 = CARTESIAN_POINT ( 'NONE',  ( 55.96859303347804371, 54.19948385550240033, 4.306917132069425946 ) ) ;
#17598 = CYLINDRICAL_SURFACE ( 'NONE', #7941, 5.000000000000007994 ) ;
#17599 = CARTESIAN_POINT ( 'NONE',  ( 56.79116909180255135, 49.79948385550240175, -4.963592699179005585 ) ) ;
#17600 = CARTESIAN_POINT ( 'NONE',  ( 56.66441430157294690, 46.90051614449765793, -2.141517661632166281 ) ) ;
#17601 = VECTOR ( 'NONE', #6514, 1000.000000000000000 ) ;
#17602 = FACE_OUTER_BOUND ( 'NONE', #17633, .T. ) ;
#17603 = CIRCLE ( 'NONE', #16971, 3.299999999999999822 ) ;
#17604 = VERTEX_POINT ( 'NONE', #10764 ) ;
#17605 = MECHANICAL_DESIGN_GEOMETRIC_PRESENTATION_REPRESENTATION (  '', ( #1940 ), #18240 ) ;
#17606 = ORIENTED_EDGE ( 'NONE', *, *, #15886, .T. ) ;
#17607 = DIRECTION ( 'NONE',  ( 0.000000000000000000, 0.000000000000000000, -1.000000000000000000 ) ) ;
#17608 = ORIENTED_EDGE ( 'NONE', *, *, #16471, .T. ) ;
#17609 = CARTESIAN_POINT ( 'NONE',  ( -1.250000000000000000, -6.429618962271402616, 0.000000000000000000 ) ) ;
#17610 = ORIENTED_EDGE ( 'NONE', *, *, #18164, .F. ) ;
#17611 = CARTESIAN_POINT ( 'NONE',  ( -14.86289650954790886, -6.617387872822862782, -9.000000000000000000 ) ) ;
#17612 = EDGE_CURVE ( 'NONE', #16121, #1649, #9290, .T. ) ;
#17613 = ORIENTED_EDGE ( 'NONE', *, *, #4959, .T. ) ;
#17614 = DIRECTION ( 'NONE',  ( -1.000000000000000000, -0.000000000000000000, 0.000000000000000000 ) ) ;
#17615 = ORIENTED_EDGE ( 'NONE', *, *, #19377, .T. ) ;
#17616 = CARTESIAN_POINT ( 'NONE',  ( 42.39856655714566358, 60.89948385550241028, 2.493737253992119207 ) ) ;
#17617 = CYLINDRICAL_SURFACE ( 'NONE', #6371, 0.7500000000000002220 ) ;
#17618 = EDGE_CURVE ( 'NONE', #14876, #2713, #5985, .T. ) ;
#17619 = PRODUCT_DEFINITION_SHAPE ( 'NONE', 'NONE',  #19430 ) ;
#17620 = CARTESIAN_POINT ( 'NONE',  ( 51.92680522751233951, 53.59948385550240602, -6.007379884777223289 ) ) ;
#17621 = CARTESIAN_POINT ( 'NONE',  ( 62.49999999999998579, 32.50000000000001421, -15.00000000000000000 ) ) ;
#17622 = VECTOR ( 'NONE', #11531, 1000.000000000000000 ) ;
#17623 = CARTESIAN_POINT ( 'NONE',  ( 73.00000000000002842, -1.000000000000000000, 6.000000000000001776 ) ) ;
#17624 = CARTESIAN_POINT ( 'NONE',  ( 52.62207051974829852, 44.60051614449766078, -7.992620115222797139 ) ) ;
#17625 = CARTESIAN_POINT ( 'NONE',  ( 44.30067958973594955, 46.10051614449766078, -1.875703265242155693 ) ) ;
#17626 = CARTESIAN_POINT ( 'NONE',  ( 45.60000000000000142, 2.789133085058097101E-16, -2.055000000000000160 ) ) ;
#17627 = CARTESIAN_POINT ( 'NONE',  ( -54.99999999999996447, -22.99999999999998579, -15.00000000000000000 ) ) ;
#17628 = ORIENTED_EDGE ( 'NONE', *, *, #12425, .F. ) ;
#17629 = AXIS2_PLACEMENT_3D ( 'NONE', #19094, #8484, #14462 ) ;
#17630 = ORIENTED_EDGE ( 'NONE', *, *, #10462, .F. ) ;
#17631 = CARTESIAN_POINT ( 'NONE',  ( -3.175194142252219631, -0.2536549670829672531, 0.000000000000000000 ) ) ;
#17632 = SURFACE_STYLE_USAGE ( .BOTH. , #2636 ) ;
#17633 = EDGE_LOOP ( 'NONE', ( #14457, #18530, #18837, #7633, #5550 ) ) ;
#17634 = CARTESIAN_POINT ( 'NONE',  ( 47.70284917648453415, 55.39948385550238896, -6.992620115222774047 ) ) ;
#17635 = DIRECTION ( 'NONE',  ( 0.000000000000000000, 0.000000000000000000, 1.000000000000000000 ) ) ;
#17636 = ORIENTED_EDGE ( 'NONE', *, *, #6302, .T. ) ;
#17637 = ORIENTED_EDGE ( 'NONE', *, *, #8435, .F. ) ;
#17638 = DIRECTION ( 'NONE',  ( -0.000000000000000000, -0.000000000000000000, 1.000000000000000000 ) ) ;
#17639 = CARTESIAN_POINT ( 'NONE',  ( -150.9999999999999432, -14.99999999999999645, 17.00000000000000000 ) ) ;
#17640 = ORIENTED_EDGE ( 'NONE', *, *, #9632, .T. ) ;
#17641 = CARTESIAN_POINT ( 'NONE',  ( 1.249999999999997558, 0.000000000000000000, 0.000000000000000000 ) ) ;
#17642 = ORIENTED_EDGE ( 'NONE', *, *, #12984, .T. ) ;
#17643 = CARTESIAN_POINT ( 'NONE',  ( -3.455068668934486276, 2.624017327439035707, -3.316620875263955437 ) ) ;
#17644 = CARTESIAN_POINT ( 'NONE',  ( 54.13287192849676188, 52.29948385550240886, 5.649768623646098220 ) ) ;
#17645 = DIRECTION ( 'NONE',  ( -0.000000000000000000, -0.000000000000000000, -1.000000000000000000 ) ) ;
#17646 = CARTESIAN_POINT ( 'NONE',  ( 45.90387839640208512, 46.30051614449766362, -5.676469297603124353 ) ) ;
#17647 = DIRECTION ( 'NONE',  ( -0.000000000000000000, -0.000000000000000000, 1.000000000000000000 ) ) ;
#17648 = PRODUCT_DEFINITION_FORMATION_WITH_SPECIFIED_SOURCE ( 'ANY', '', #4297, .NOT_KNOWN. ) ;
#17649 = DIRECTION ( 'NONE',  ( 0.000000000000000000, 0.000000000000000000, -1.000000000000000000 ) ) ;
#17650 = ORIENTED_EDGE ( 'NONE', *, *, #9630, .F. ) ;
#17651 = ORIENTED_EDGE ( 'NONE', *, *, #19014, .F. ) ;
#17652 = LINE ( 'NONE', #4203, #16245 ) ;
#17653 = CARTESIAN_POINT ( 'NONE',  ( 1.250000000000000000, -6.429618962271402616, -1.000000000000000000 ) ) ;
#17654 = ORIENTED_EDGE ( 'NONE', *, *, #16858, .T. ) ;
#17655 = CARTESIAN_POINT ( 'NONE',  ( 0.000000000000000000, 0.000000000000000000, -4.694516984716113228 ) ) ;
#17656 = ADVANCED_FACE ( 'NONE', ( #7445 ), #16475, .F. ) ;
#17657 = ORIENTED_EDGE ( 'NONE', *, *, #13363, .T. ) ;
#17658 = ORIENTED_EDGE ( 'NONE', *, *, #2592, .F. ) ;
#17659 = DIRECTION ( 'NONE',  ( 0.000000000000000000, 0.000000000000000000, -1.000000000000000000 ) ) ;
#17660 = CARTESIAN_POINT ( 'NONE',  ( 44.28664221472221385, 49.90051614449766504, 1.832500667257213722 ) ) ;
#17661 = DIRECTION ( 'NONE',  ( 0.000000000000000000, -0.8660254037844380415, 0.5000000000000012212 ) ) ;
#17662 = CARTESIAN_POINT ( 'NONE',  ( 44.88205777487398507, 49.19948385550240744, -3.688883143319540814 ) ) ;
#17663 = FACE_OUTER_BOUND ( 'NONE', #10415, .T. ) ;
#17664 = CARTESIAN_POINT ( 'NONE',  ( 47.74827507625478518, 50.59948385550238470, 7.007379884777227730 ) ) ;
#17665 = CARTESIAN_POINT ( 'NONE',  ( 50.02271294988505446, 46.50051614449766646, -8.000000000000001776 ) ) ;
#17666 = CARTESIAN_POINT ( 'NONE',  ( -0.6666666666666666297, -4.233901974057276973, -3.300726591567087365 ) ) ;
#17667 = EDGE_CURVE ( 'NONE', #6445, #9743, #10040, .T. ) ;
#17668 = VERTEX_POINT ( 'NONE', #3812 ) ;
#17669 = DIRECTION ( 'NONE',  ( 0.000000000000000000, 0.000000000000000000, 1.000000000000000000 ) ) ;
#17670 = DIRECTION ( 'NONE',  ( 0.000000000000000000, 0.000000000000000000, 1.000000000000000000 ) ) ;
#17671 = VERTEX_POINT ( 'NONE', #8301 ) ;
#17672 = DIRECTION ( 'NONE',  ( 0.000000000000000000, 0.000000000000000000, -1.000000000000000000 ) ) ;
#17673 = ADVANCED_FACE ( 'NONE', ( #7917 ), #16863, .F. ) ;
#17674 = AXIS2_PLACEMENT_3D ( 'NONE', #12575, #15420, #6315 ) ;
#17675 = EDGE_CURVE ( 'NONE', #9948, #6607, #18524, .T. ) ;
#17676 = ADVANCED_FACE ( 'NONE', ( #674 ), #4893, .F. ) ;
#17677 = DIRECTION ( 'NONE',  ( 1.000000000000000000, 0.000000000000000000, 0.000000000000000000 ) ) ;
#17678 = VECTOR ( 'NONE', #17736, 1000.000000000000000 ) ;
#17679 = EDGE_CURVE ( 'NONE', #15861, #10123, #15692, .T. ) ;
#17680 = DIRECTION ( 'NONE',  ( 1.000000000000000000, 0.000000000000000000, 0.000000000000000000 ) ) ;
#17681 = DIRECTION ( 'NONE',  ( 0.000000000000000000, 0.000000000000000000, 1.000000000000000000 ) ) ;
#17682 = LINE ( 'NONE', #4334, #4612 ) ;
#17683 = CARTESIAN_POINT ( 'NONE',  ( -1.250000000000000000, -6.429618962271402616, -1.000000000000000000 ) ) ;
#17684 = EDGE_CURVE ( 'NONE', #5943, #508, #18628, .T. ) ;
#17685 = CARTESIAN_POINT ( 'NONE',  ( 1.287237434362044075, 3.875615274277557809, -3.430618716626812059 ) ) ;
#17686 = CARTESIAN_POINT ( 'NONE',  ( 47.74827507625478518, 54.59948385550239180, 7.007379884777227730 ) ) ;
#17687 = DIRECTION ( 'NONE',  ( -1.000000000000000000, 0.000000000000000000, 0.000000000000000000 ) ) ;
#17688 = CARTESIAN_POINT ( 'NONE',  ( 57.61547081786812896, 48.09948385550240602, 2.450534656007040901 ) ) ;
#17689 = CARTESIAN_POINT ( 'NONE',  ( 2.649999999999988809, 15.00000000000001599, -15.00000000000000000 ) ) ;
#17690 = CARTESIAN_POINT ( 'NONE',  ( 43.33558569842706021, 49.90051614449766504, 2.141517661632167169 ) ) ;
#17691 =( REPRESENTATION_RELATIONSHIP ('NONE','NONE', #16703, #18081 ) REPRESENTATION_RELATIONSHIP_WITH_TRANSFORMATION ( #688 )SHAPE_REPRESENTATION_RELATIONSHIP( ) );
#17692 = DIRECTION ( 'NONE',  ( 0.000000000000000000, 0.000000000000000000, -1.000000000000000000 ) ) ;
#17693 = ORIENTED_EDGE ( 'NONE', *, *, #14071, .F. ) ;
#17694 = ORIENTED_EDGE ( 'NONE', *, *, #16002, .T. ) ;
#17695 = CARTESIAN_POINT ( 'NONE',  ( 32.00000000000000000, -1.000000000000000000, 6.000000000000001776 ) ) ;
#17696 = ORIENTED_EDGE ( 'NONE', *, *, #13865, .F. ) ;
#17697 = EDGE_CURVE ( 'NONE', #870, #7187, #14106, .T. ) ;
#17698 = EDGE_CURVE ( 'NONE', #950, #13007, #7236, .T. ) ;
#17699 = LINE ( 'NONE', #1511, #13440 ) ;
#17700 = ORIENTED_EDGE ( 'NONE', *, *, #4390, .F. ) ;
#17701 = CARTESIAN_POINT ( 'NONE',  ( -74.99999999999997158, 45.00000000000001421, -15.00000000000000000 ) ) ;
#17702 = VERTEX_POINT ( 'NONE', #5169 ) ;
#17703 = CIRCLE ( 'NONE', #10489, 3.800000000000000266 ) ;
#17704 = CARTESIAN_POINT ( 'NONE',  ( -62.49999999999997158, 32.50000000000001421, 15.00000000000000000 ) ) ;
#17705 = VERTEX_POINT ( 'NONE', #18434 ) ;
#17706 = CARTESIAN_POINT ( 'NONE',  ( 57.61547081786812896, 62.09948385550240602, 2.450534656007040901 ) ) ;
#17707 = DIRECTION ( 'NONE',  ( -0.000000000000000000, -0.000000000000000000, -1.000000000000000000 ) ) ;
#17708 = CARTESIAN_POINT ( 'NONE',  ( 55.69932041026404335, 51.89948385550241028, -1.875703265242203432 ) ) ;
#17709 = CARTESIAN_POINT ( 'NONE',  ( 4.175813232069148562, -2.061359961916374051, -3.570380186727397653 ) ) ;
#17710 = FACE_OUTER_BOUND ( 'NONE', #9177, .T. ) ;
#17711 = CARTESIAN_POINT ( 'NONE',  ( 45.27934281921082516, 45.70051614449766220, 6.458785618021089192 ) ) ;
#17712 = COLOUR_RGB ( '',1.000000000000000000, 0.9490196078431372140, 0.9098039215686274384 ) ;
#17713 = CARTESIAN_POINT ( 'NONE',  ( 48.07319477248762496, 48.40051614449766504, -6.007379884777208190 ) ) ;
#17714 = CYLINDRICAL_SURFACE ( 'NONE', #5675, 24.99999999999999289 ) ;
#17715 = CARTESIAN_POINT ( 'NONE',  ( -0.1374368770859597522, -4.808326913195983821, 0.000000000000000000 ) ) ;
#17716 = VERTEX_POINT ( 'NONE', #4981 ) ;
#17717 = ORIENTED_EDGE ( 'NONE', *, *, #16950, .F. ) ;
#17718 = DIRECTION ( 'NONE',  ( 1.000000000000000000, 0.000000000000000000, 0.000000000000000000 ) ) ;
#17719 = EDGE_LOOP ( 'NONE', ( #17502, #3899, #10065, #4348 ) ) ;
#17720 = ADVANCED_FACE ( 'NONE', ( #3709 ), #8557, .T. ) ;
#17721 = CARTESIAN_POINT ( 'NONE',  ( -154.9999999999999716, -23.00000000000000000, -10.00000000000000000 ) ) ;
#17722 = EDGE_CURVE ( 'NONE', #11109, #3030, #3180, .T. ) ;
#17723 = EDGE_LOOP ( 'NONE', ( #1369, #14267, #13360, #4547, #17163 ) ) ;
#17724 = ORIENTED_EDGE ( 'NONE', *, *, #10992, .T. ) ;
#17725 = DIRECTION ( 'NONE',  ( 0.000000000000000000, 0.000000000000000000, 1.000000000000000000 ) ) ;
#17726 = VECTOR ( 'NONE', #10974, 1000.000000000000000 ) ;
#17727 = DIRECTION ( 'NONE',  ( 0.000000000000000000, 0.000000000000000000, 1.000000000000000000 ) ) ;
#17728 = ADVANCED_FACE ( 'NONE', ( #10799 ), #9050, .F. ) ;
#17729 = ORIENTED_EDGE ( 'NONE', *, *, #13610, .F. ) ;
#17730 = DIRECTION ( 'NONE',  ( 1.000000000000000000, 0.000000000000000000, 0.000000000000000000 ) ) ;
#17731 = VERTEX_POINT ( 'NONE', #4837 ) ;
#17732 = DIRECTION ( 'NONE',  ( -0.000000000000000000, -0.000000000000000000, 1.000000000000000000 ) ) ;
#17733 = CARTESIAN_POINT ( 'NONE',  ( 57.36023556966787851, 49.99948385550238328, -0.02388180880522424582 ) ) ;
#17734 = CARTESIAN_POINT ( 'NONE',  ( -4.000000000000000000, 0.000000000000000000, 0.000000000000000000 ) ) ;
#17735 = CARTESIAN_POINT ( 'NONE',  ( 43.34962307344078880, 48.10051614449766078, -2.184720259617096705 ) ) ;
#17736 = DIRECTION ( 'NONE',  ( -0.000000000000000000, -0.000000000000000000, -1.000000000000000000 ) ) ;
#17737 = DIRECTION ( 'NONE',  ( 1.000000000000000000, 0.000000000000000000, 0.000000000000000000 ) ) ;
#17738 = CARTESIAN_POINT ( 'NONE',  ( 1.171083334267915221, -24.65495046420793201, 9.999999999999998224 ) ) ;
#17739 = EDGE_CURVE ( 'NONE', #3362, #1643, #19164, .T. ) ;
#17740 = EDGE_LOOP ( 'NONE', ( #16125, #10801, #3382, #685, #5844, #14166, #17989, #18310 ) ) ;
#17741 = VERTEX_POINT ( 'NONE', #12184 ) ;
#17742 = CARTESIAN_POINT ( 'NONE',  ( -2.649999999999988365, 15.00000000000001599, 15.00000000000000000 ) ) ;
#17743 = EDGE_CURVE ( 'NONE', #6553, #10315, #9234, .T. ) ;
#17744 = CARTESIAN_POINT ( 'NONE',  ( 43.34962307344081012, 46.89948385550240317, 2.184720259617164650 ) ) ;
#17745 = CIRCLE ( 'NONE', #12072, 4.872650870659752442 ) ;
#17746 = DIRECTION ( 'NONE',  ( -0.000000000000000000, -0.000000000000000000, 1.000000000000000000 ) ) ;
#17747 = ORIENTED_EDGE ( 'NONE', *, *, #3643, .T. ) ;
#17748 = DIRECTION ( 'NONE',  ( 0.000000000000000000, 0.000000000000000000, -1.000000000000000000 ) ) ;
#17749 = ORIENTED_EDGE ( 'NONE', *, *, #15081, .F. ) ;
#17750 = VERTEX_POINT ( 'NONE', #1902 ) ;
#17751 = AXIS2_PLACEMENT_3D ( 'NONE', #11858, #7555, #4620 ) ;
#17752 = FACE_OUTER_BOUND ( 'NONE', #13368, .T. ) ;
#17753 = UNCERTAINTY_MEASURE_WITH_UNIT (LENGTH_MEASURE( 1.000000000000000082E-05 ), #3035, 'distance_accuracy_value', 'NONE');
#17754 = CARTESIAN_POINT ( 'NONE',  ( 17.79870116617256315, -29.12174527145368330, -9.000000000000000000 ) ) ;
#17755 = CARTESIAN_POINT ( 'NONE',  ( 55.69932041026405045, 47.10051614449766078, 1.875703265242156359 ) ) ;
#17756 = CARTESIAN_POINT ( 'NONE',  ( -1.149999999999998135, 0.000000000000000000, 0.000000000000000000 ) ) ;
#17757 = LINE ( 'NONE', #8824, #4587 ) ;
#17758 = CARTESIAN_POINT ( 'NONE',  ( 44.88205777487398507, 59.19948385550240744, -3.688883143319540814 ) ) ;
#17759 = CARTESIAN_POINT ( 'NONE',  ( -154.9999999999999716, -14.99999999999999645, 10.00000000000000000 ) ) ;
#17760 = CARTESIAN_POINT ( 'NONE',  ( 44.03140696652192787, 55.19948385550238612, -4.306917132069425058 ) ) ;
#17761 = CARTESIAN_POINT ( 'NONE',  ( 57.61547081786810764, 44.90051614449765793, -2.450534656007114176 ) ) ;
#17762 = CARTESIAN_POINT ( 'NONE',  ( 4.124214193018069352, -2.028338413290947440, -3.513185186763551737 ) ) ;
#17763 = VECTOR ( 'NONE', #427, 1000.000000000000000 ) ;
#17764 = LINE ( 'NONE', #2962, #3085 ) ;
#17765 = VECTOR ( 'NONE', #5962, 1000.000000000000000 ) ;
#17766 = PRODUCT_CONTEXT ( 'NONE', #17808, 'mechanical' ) ;
#17767 = VERTEX_POINT ( 'NONE', #1804 ) ;
#17768 = CARTESIAN_POINT ( 'NONE',  ( 5.000000000000003553, -20.00000000000000000, 15.00000000000000355 ) ) ;
#17769 = CLOSED_SHELL ( 'NONE', ( #17069, #4132, #1270, #18041, #9395, #3431, #14525, #15744, #6278, #1157, #13212, #7656, #5667, #14437, #12766, #1069, #8796, #10815, #3738, #4009, #16300, #4954, #105, #19154 ) ) ;
#17770 = CARTESIAN_POINT ( 'NONE',  ( 2.449293598294706513E-15, -20.00000000000000000, -9.000000000000000000 ) ) ;
#17771 = CIRCLE ( 'NONE', #13683, 20.00000000000000000 ) ;
#17772 = CARTESIAN_POINT ( 'NONE',  ( 6.371506350351447523, -5.409331239960139648, -0.8483282427581471108 ) ) ;
#17773 = CARTESIAN_POINT ( 'NONE',  ( 3.309651814758565180, -5.455921364805393026, 0.000000000000000000 ) ) ;
#17774 = CARTESIAN_POINT ( 'NONE',  ( -54.99999999999996447, -14.99999999999998579, 15.00000000000000000 ) ) ;
#17775 = CIRCLE ( 'NONE', #13703, 0.5999999999999998668 ) ;
#17776 = CARTESIAN_POINT ( 'NONE',  ( 8.500000000000000000, 0.000000000000000000, 4.000000000000000000 ) ) ;
#17777 = DIRECTION ( 'NONE',  ( -0.9995917534020515305, -0.02857142857142857054, 0.000000000000000000 ) ) ;
#17778 = CARTESIAN_POINT ( 'NONE',  ( 54.09612160359786515, 53.69948385550240744, -5.676469297603166098 ) ) ;
#17779 = CARTESIAN_POINT ( 'NONE',  ( -65.14999999999996305, 32.50000000000001421, 10.00000000000000000 ) ) ;
#17780 = CARTESIAN_POINT ( 'NONE',  ( 52.57664461997811856, 51.59948385550240602, -8.007379884777229506 ) ) ;
#17781 = CARTESIAN_POINT ( 'NONE',  ( -19.99999999999999289, -14.99999999999998579, -23.00000000000000000 ) ) ;
#17782 = EDGE_CURVE ( 'NONE', #19337, #19038, #9242, .T. ) ;
#17783 = CARTESIAN_POINT ( 'NONE',  ( 55.96859303347802239, 50.80051614449766362, -4.306917132069484566 ) ) ;
#17784 = VECTOR ( 'NONE', #9221, 1000.000000000000000 ) ;
#17785 = LINE ( 'NONE', #6020, #11272 ) ;
#17786 = VERTEX_POINT ( 'NONE', #3850 ) ;
#17787 = EDGE_CURVE ( 'NONE', #17949, #8729, #11087, .T. ) ;
#17788 = VECTOR ( 'NONE', #1685, 1000.000000000000000 ) ;
#17789 = EDGE_LOOP ( 'NONE', ( #12490, #11735, #11621, #9074 ) ) ;
#17790 = DIRECTION ( 'NONE',  ( 1.000000000000000000, 0.000000000000000000, 0.000000000000000000 ) ) ;
#17791=STYLED_ITEM('',(#19468),#8790);
#17792 = ORIENTED_EDGE ( 'NONE', *, *, #3531, .F. ) ;
#17793 = EDGE_CURVE ( 'NONE', #8318, #2946, #4696, .T. ) ;
#17794 = EDGE_CURVE ( 'NONE', #10823, #2682, #1245, .T. ) ;
#17795 = DIRECTION ( 'NONE',  ( 1.000000000000000000, 0.000000000000000000, 0.000000000000000000 ) ) ;
#17796 = ORIENTED_EDGE ( 'NONE', *, *, #10211, .T. ) ;
#17797 = CYLINDRICAL_SURFACE ( 'NONE', #11282, 0.9999999999999991118 ) ;
#17798 = EDGE_CURVE ( 'NONE', #14027, #3339, #15332, .T. ) ;
#17799 = EDGE_LOOP ( 'NONE', ( #13286, #5254 ) ) ;
#17800 = CARTESIAN_POINT ( 'NONE',  ( 20.00000000000000000, -25.00000000000000711, -23.00000000000000000 ) ) ;
#17801 = ORIENTED_EDGE ( 'NONE', *, *, #6332, .F. ) ;
#17802 = CARTESIAN_POINT ( 'NONE',  ( 50.02271294988513972, 62.49948385550240459, 8.000000000000001776 ) ) ;
#17803 = CARTESIAN_POINT ( 'NONE',  ( 0.000000000000000000, 0.000000000000000000, -1.000000000000000000 ) ) ;
#17804 = AXIS2_PLACEMENT_3D ( 'NONE', #13724, #303, #12253 ) ;
#17805 = CARTESIAN_POINT ( 'NONE',  ( 53.50833635130540955, 59.69948385550240744, -4.867452303228209765 ) ) ;
#17806 = CARTESIAN_POINT ( 'NONE',  ( 17.32050807568866091, -9.999999999999797495, -9.000000000000000000 ) ) ;
#17807 = DIRECTION ( 'NONE',  ( -0.2439756946365075896, 0.9697813467099856144, 1.610118993450814692E-22 ) ) ;
#17808 = APPLICATION_CONTEXT ( 'automotive_design' ) ;
#17809 = CARTESIAN_POINT ( 'NONE',  ( 54.72065718078918906, 52.70051614449766220, -6.458785618021089192 ) ) ;
#17810 = EDGE_CURVE ( 'NONE', #3228, #16268, #2190, .T. ) ;
#17811 = CARTESIAN_POINT ( 'NONE',  ( 51.97223112728249816, 50.60051614449765367, -5.992620115222793586 ) ) ;
#17812 = EDGE_CURVE ( 'NONE', #3235, #3752, #4381, .T. ) ;
#17813 = DIRECTION ( 'NONE',  ( 0.000000000000000000, 0.000000000000000000, 1.000000000000000000 ) ) ;
#17814 = DIRECTION ( 'NONE',  ( -1.000000000000000000, 0.000000000000000000, 0.000000000000000000 ) ) ;
#17815 = ORIENTED_EDGE ( 'NONE', *, *, #4368, .F. ) ;
#17816 = ORIENTED_EDGE ( 'NONE', *, *, #2723, .T. ) ;
#17817 = DIRECTION ( 'NONE',  ( -0.000000000000000000, -0.000000000000000000, 1.000000000000000000 ) ) ;
#17818 = ORIENTED_EDGE ( 'NONE', *, *, #8553, .T. ) ;
#17819 = COLOUR_RGB ( '',0.8941176470588234615, 0.8941176470588234615, 0.8941176470588234615 ) ;
#17820 = AXIS2_PLACEMENT_3D ( 'NONE', #6043, #1530, #4377 ) ;
#17821 = CARTESIAN_POINT ( 'NONE',  ( 54.09612160359786515, 61.69948385550240744, -5.676469297603166098 ) ) ;
#17822 = DIRECTION ( 'NONE',  ( 0.000000000000000000, 0.000000000000000000, 1.000000000000000000 ) ) ;
#17823 = ORIENTED_EDGE ( 'NONE', *, *, #3348, .F. ) ;
#17824 = CARTESIAN_POINT ( 'NONE',  ( 0.000000000000000000, 0.000000000000000000, -1.000000000000000000 ) ) ;
#17825 = CARTESIAN_POINT ( 'NONE',  ( 52.29715082351547295, 48.39948385550240317, 6.992620115222774047 ) ) ;
#17826 = VERTEX_POINT ( 'NONE', #8049 ) ;
#17827 = FACE_OUTER_BOUND ( 'NONE', #13196, .T. ) ;
#17828 = VERTEX_POINT ( 'NONE', #3947 ) ;
#17829 = DIRECTION ( 'NONE',  ( 0.000000000000000000, 0.000000000000000000, -1.000000000000000000 ) ) ;
#17830 = CARTESIAN_POINT ( 'NONE',  ( 43.33558569842703179, 59.09948385550240602, -2.141517661632099223 ) ) ;
#17831 = FACE_OUTER_BOUND ( 'NONE', #17789, .T. ) ;
#17832 = CARTESIAN_POINT ( 'NONE',  ( 47.70284917648459100, 45.60051614449765367, 6.992620115222796251 ) ) ;
#17833 = DIRECTION ( 'NONE',  ( 0.000000000000000000, 0.000000000000000000, 1.000000000000000000 ) ) ;
#17834 = VECTOR ( 'NONE', #18428, 1000.000000000000000 ) ;
#17835 = VECTOR ( 'NONE', #15630, 1000.000000000000000 ) ;
#17836 = CARTESIAN_POINT ( 'NONE',  ( 1.249999999999997780, 5.021051876504148371E-16, 4.100000000000000533 ) ) ;
#17837 = CARTESIAN_POINT ( 'NONE',  ( -4.000000000000000000, -0.8382240730041925492, -3.220610619767135141 ) ) ;
#17838 = ORIENTED_EDGE ( 'NONE', *, *, #13247, .T. ) ;
#17839 = AXIS2_PLACEMENT_3D ( 'NONE', #5205, #11570, #8440 ) ;
#17840 = VERTEX_POINT ( 'NONE', #8153 ) ;
#17841 = ORIENTED_EDGE ( 'NONE', *, *, #5704, .F. ) ;
#17842 = CARTESIAN_POINT ( 'NONE',  ( -1.654252653721913102, -3.663718938583024443, -0.01223254789874440342 ) ) ;
#17843 =( NAMED_UNIT ( * ) SI_UNIT ( $, .STERADIAN. ) SOLID_ANGLE_UNIT ( ) );
#17844 = CARTESIAN_POINT ( 'NONE',  ( 45.27934281921075410, 65.29948385550241596, -6.458785618021043895 ) ) ;
#17845 = DIRECTION ( 'NONE',  ( 1.000000000000000000, 0.000000000000000000, 0.000000000000000000 ) ) ;
#17846 = EDGE_LOOP ( 'NONE', ( #8832, #18213, #7813, #1316 ) ) ;
#17847 = DIRECTION ( 'NONE',  ( -1.000000000000000000, 0.000000000000000000, 0.000000000000000000 ) ) ;
#17848 = AXIS2_PLACEMENT_3D ( 'NONE', #10510, #17795, #8569 ) ;
#17849 = CIRCLE ( 'NONE', #9364, 2.649999999999985700 ) ;
#17850 = ORIENTED_EDGE ( 'NONE', *, *, #10811, .F. ) ;
#17851 = VERTEX_POINT ( 'NONE', #12571 ) ;
#17852 = ADVANCED_FACE ( 'NONE', ( #14429 ), #12464, .T. ) ;
#17853 = CARTESIAN_POINT ( 'NONE',  ( 6.371506350351443082, -3.439339428956426747, 4.260454149911180544 ) ) ;
#17854 = DIRECTION ( 'NONE',  ( 0.000000000000000000, 0.000000000000000000, 1.000000000000000000 ) ) ;
#17855 = AXIS2_PLACEMENT_3D ( 'NONE', #8549, #14517, #18963 ) ;
#17856 = CARTESIAN_POINT ( 'NONE',  ( 48.07319477248762496, 46.40051614449765793, -6.007379884777208190 ) ) ;
#17857 = DIRECTION ( 'NONE',  ( -0.000000000000000000, -0.000000000000000000, 1.000000000000000000 ) ) ;
#17858 = EDGE_CURVE ( 'NONE', #11648, #18236, #5025, .T. ) ;
#17859 = DIRECTION ( 'NONE',  ( -0.1045284632676563297, 0.9945218953682731788, 0.000000000000000000 ) ) ;
#17860 = CARTESIAN_POINT ( 'NONE',  ( 53.54508667620428497, 56.29948385550240886, 4.840751629271157874 ) ) ;
#17861 = DIRECTION ( 'NONE',  ( 1.000000000000000000, 0.000000000000000000, 0.000000000000000000 ) ) ;
#17862 = CARTESIAN_POINT ( 'NONE',  ( 56.65037692655918988, 51.89948385550241028, -2.184720259617163762 ) ) ;
#17863 = VECTOR ( 'NONE', #8839, 1000.000000000000000 ) ;
#17864 = CARTESIAN_POINT ( 'NONE',  ( 56.81924384183006538, 56.80051614449764941, -4.924951120819380357 ) ) ;
#17865 = DIRECTION ( 'NONE',  ( -0.8571673013836855759, 0.000000000000000000, -0.5150380737757258576 ) ) ;
#17866 = CARTESIAN_POINT ( 'NONE',  ( -4.211140560182196957, 2.431303136016537803, -3.745885042887433514 ) ) ;
#17867 = DIRECTION ( 'NONE',  ( 0.000000000000000000, 0.000000000000000000, 1.000000000000000000 ) ) ;
#17868 =( LENGTH_UNIT ( ) NAMED_UNIT ( * ) SI_UNIT ( .MILLI., .METRE. ) );
#17869 = B_SPLINE_CURVE_WITH_KNOTS ( 'NONE', 3,
 ( #15075, #3593, #2231, #11122, #9554, #15545, #10930, #18801, #8378, #13963, #3788, #8278, #18702, #4957, #2124, #8190 ),
 .UNSPECIFIED., .F., .F.,
 ( 4, 3, 3, 3, 3, 4 ),
 ( -2.111273352579798197E-06, 0.000000000000000000, 3.519286887794736512E-05, 7.191842652068568460E-05, 0.0001049868727093669315, 0.0001382836236822145742 ),
 .UNSPECIFIED. ) ;
#17870 = DIRECTION ( 'NONE',  ( 0.9931793912140981506, 0.1165962986873662205, 0.000000000000000000 ) ) ;
#17871 = CIRCLE ( 'NONE', #14397, 20.00000000000000000 ) ;
#17872 = EDGE_LOOP ( 'NONE', ( #5621, #16223, #5426, #5157 ) ) ;
#17873 = DIRECTION ( 'NONE',  ( -0.000000000000000000, -0.000000000000000000, 1.000000000000000000 ) ) ;
#17874 = CARTESIAN_POINT ( 'NONE',  ( 2.000000000000000000, 0.8865213383406680414, -1.535500000000000975 ) ) ;
#17875 = AXIS2_PLACEMENT_3D ( 'NONE', #11068, #4997, #11629 ) ;
#17876 = DIRECTION ( 'NONE',  ( 1.000000000000000000, 0.000000000000000000, 0.000000000000000000 ) ) ;
#17877 = CIRCLE ( 'NONE', #13154, 8.000000000000007105 ) ;
#17878 = DIRECTION ( 'NONE',  ( 0.000000000000000000, 0.000000000000000000, -1.000000000000000000 ) ) ;
#17879 = CARTESIAN_POINT ( 'NONE',  ( 0.000000000000000000, 0.000000000000000000, -0.8000000000000000444 ) ) ;
#17880 = DIRECTION ( 'NONE',  ( 1.000000000000000000, -0.000000000000000000, -0.000000000000000000 ) ) ;
#17881 = CARTESIAN_POINT ( 'NONE',  ( 44.05948171654949874, 58.79948385550240886, 4.345558710429105354 ) ) ;
#17882 = AXIS2_PLACEMENT_3D ( 'NONE', #10121, #19376, #11591 ) ;
#17883 = DIRECTION ( 'NONE',  ( -1.000000000000000000, 0.000000000000000000, 0.000000000000000000 ) ) ;
#17884 = CARTESIAN_POINT ( 'NONE',  ( 45.27934281921075410, 53.29948385550240886, -6.458785618021043895 ) ) ;
#17885 = DIRECTION ( 'NONE',  ( 1.000000000000000000, 0.000000000000000000, 0.000000000000000000 ) ) ;
#17886 = CARTESIAN_POINT ( 'NONE',  ( 52.29715082351538769, 56.60051614449766788, -6.992620115222796251 ) ) ;
#17887 = DIRECTION ( 'NONE',  ( 1.000000000000000000, 0.000000000000000000, 0.000000000000000000 ) ) ;
#17888 = AXIS2_PLACEMENT_3D ( 'NONE', #5781, #2667, #8620 ) ;
#17889 = VERTEX_POINT ( 'NONE', #18476 ) ;
#17890 = VECTOR ( 'NONE', #11513, 1000.000000000000000 ) ;
#17891 = VECTOR ( 'NONE', #3810, 1000.000000000000000 ) ;
#17892 = EDGE_LOOP ( 'NONE', ( #89, #16663, #5776, #11227 ) ) ;
#17893 = DIRECTION ( 'NONE',  ( 1.000000000000000000, 0.000000000000000000, 0.000000000000000000 ) ) ;
#17894 = ORIENTED_EDGE ( 'NONE', *, *, #2152, .F. ) ;
#17895 = VECTOR ( 'NONE', #15526, 1000.000000000000000 ) ;
#17896 = DIRECTION ( 'NONE',  ( 0.000000000000000000, 0.000000000000000000, 1.000000000000000000 ) ) ;
#17897 = ORIENTED_EDGE ( 'NONE', *, *, #6694, .F. ) ;
#17898 = DIRECTION ( 'NONE',  ( 0.000000000000000000, 0.000000000000000000, 1.000000000000000000 ) ) ;
#17899 = EDGE_CURVE ( 'NONE', #1343, #8396, #14128, .T. ) ;
#17900 = ORIENTED_EDGE ( 'NONE', *, *, #7350, .F. ) ;
#17901 = CARTESIAN_POINT ( 'NONE',  ( 14.17539641854900978, -5.891203581559908642, -9.000000000000000000 ) ) ;
#17902 = ORIENTED_EDGE ( 'NONE', *, *, #12626, .F. ) ;
#17903 = CARTESIAN_POINT ( 'NONE',  ( -0.1481481481481481122, -4.797713218419819903, -1.000000000000000000 ) ) ;
#17904 = FACE_BOUND ( 'NONE', #11013, .T. ) ;
#17905 = CARTESIAN_POINT ( 'NONE',  ( 53.54508667620428497, 58.29948385550240886, 4.840751629271157874 ) ) ;
#17906 = DIRECTION ( 'NONE',  ( -1.000000000000000000, 0.000000000000000000, -0.000000000000000000 ) ) ;
#17907 = CARTESIAN_POINT ( 'NONE',  ( 20.00000000000000000, -20.00000000000000000, -23.00000000000000000 ) ) ;
#17908 = AXIS2_PLACEMENT_3D ( 'NONE', #12150, #10287, #19246 ) ;
#17909 = CARTESIAN_POINT ( 'NONE',  ( 49.97728705011495265, 53.50051614449767357, 8.000000000000001776 ) ) ;
#17910 = CARTESIAN_POINT ( 'NONE',  ( 48.02776887271750184, 47.60051614449766078, 5.992620115222795363 ) ) ;
#17911 = AXIS2_PLACEMENT_3D ( 'NONE', #3177, #11980, #220 ) ;
#17912 = PLANE ( 'NONE',  #11924 ) ;
#17913 = PLANE ( 'NONE',  #15343 ) ;
#17914 = VERTEX_POINT ( 'NONE', #10998 ) ;
#17915 = EDGE_CURVE ( 'NONE', #7311, #14352, #7827, .T. ) ;
#17916 = EDGE_LOOP ( 'NONE', ( #10551, #6540, #750, #14446 ) ) ;
#17917 = CARTESIAN_POINT ( 'NONE',  ( 2.000000000000005329, -3.464101615137751722, 0.000000000000000000 ) ) ;
#17918 = ORIENTED_EDGE ( 'NONE', *, *, #18385, .T. ) ;
#17919 = APPLICATION_CONTEXT ( 'automotive_design' ) ;
#17920 = CARTESIAN_POINT ( 'NONE',  ( 56.65037692655918988, 63.89948385550239607, -2.184720259617163762 ) ) ;
#17921 = VERTEX_POINT ( 'NONE', #8248 ) ;
#17922 = LINE ( 'NONE', #16445, #18825 ) ;
#17923 = PRODUCT ( 'reel holder', 'reel holder', '', ( #1483 ) ) ;
#17924 = EDGE_CURVE ( 'NONE', #1565, #17851, #2521, .T. ) ;
#17925 = CARTESIAN_POINT ( 'NONE',  ( 45.90387839640214196, 46.69948385550240744, 5.676469297603166098 ) ) ;
#17926 = AXIS2_PLACEMENT_3D ( 'NONE', #78, #4870, #12214 ) ;
#17927 = EDGE_CURVE ( 'NONE', #5450, #5403, #5967, .T. ) ;
#17928 = ORIENTED_EDGE ( 'NONE', *, *, #12398, .T. ) ;
#17929 = CARTESIAN_POINT ( 'NONE',  ( 0.4472135954999577612, 0.000000000000000000, 0.000000000000000000 ) ) ;
#17930 = ORIENTED_EDGE ( 'NONE', *, *, #4050, .T. ) ;
#17931 = CARTESIAN_POINT ( 'NONE',  ( 52.57664461997811856, 49.59948385550241312, -8.007379884777229506 ) ) ;
#17932 = CARTESIAN_POINT ( 'NONE',  ( 53.93078149122418807, 45.00000000000000000, -5.235029531081472953 ) ) ;
#17933 = CARTESIAN_POINT ( 'NONE',  ( 52.29715082351547295, 60.39948385550239607, 6.992620115222774047 ) ) ;
#17934 = CARTESIAN_POINT ( 'NONE',  ( 6.534838248920897819, 2.951765777552412651, 5.112608298763836601 ) ) ;
#17935 = CARTESIAN_POINT ( 'NONE',  ( -2.000000000000000000, -6.429618962271402616, 0.000000000000000000 ) ) ;
#17936 = CARTESIAN_POINT ( 'NONE',  ( 55.96859303347802239, 52.80051614449764941, -4.306917132069484566 ) ) ;
#17937 = DIRECTION ( 'NONE',  ( 1.000000000000000000, 0.000000000000000000, -0.000000000000000000 ) ) ;
#17938 = EDGE_CURVE ( 'NONE', #3703, #5826, #8967, .T. ) ;
#17939 = CARTESIAN_POINT ( 'NONE',  ( -54.99999999999996447, -6.999999999999985789, -15.00000000000000000 ) ) ;
#17940 = ADVANCED_FACE ( 'NONE', ( #13249 ), #14715, .T. ) ;
#17941 = CARTESIAN_POINT ( 'NONE',  ( -4.000000000000000000, -0.8232339106130515116, -3.430630286862743183 ) ) ;
#17942 = VERTEX_POINT ( 'NONE', #4441 ) ;
#17943 = EDGE_CURVE ( 'NONE', #2689, #9187, #4785, .T. ) ;
#17944 = ORIENTED_EDGE ( 'NONE', *, *, #10684, .T. ) ;
#17945 = ORIENTED_EDGE ( 'NONE', *, *, #3222, .F. ) ;
#17946 = CARTESIAN_POINT ( 'NONE',  ( -0.3198814748697807464, -4.434118497892185040, -0.3507732604232532969 ) ) ;
#17947 = CARTESIAN_POINT ( 'NONE',  ( 43.33558569842703179, 47.09948385550240602, -2.141517661632099223 ) ) ;
#17948 = DIRECTION ( 'NONE',  ( 0.000000000000000000, -0.000000000000000000, 1.000000000000000000 ) ) ;
#17949 = VERTEX_POINT ( 'NONE', #5711 ) ;
#17950 = CARTESIAN_POINT ( 'NONE',  ( 1.149999999999998135, 5.021051876504148371E-16, 4.100000000000000533 ) ) ;
#17951 = ORIENTED_EDGE ( 'NONE', *, *, #4076, .F. ) ;
#17952 = CARTESIAN_POINT ( 'NONE',  ( 47.74827507625470702, 56.40051614449766504, -7.007379884777204637 ) ) ;
#17953 = EDGE_LOOP ( 'NONE', ( #6232, #6206, #18398, #1360 ) ) ;
#17954 = B_SPLINE_CURVE_WITH_KNOTS ( 'NONE', 3,
 ( #19048, #10096, #5696, #15992, #18951, #5491 ),
 .UNSPECIFIED., .F., .F.,
 ( 4, 2, 4 ),
 ( 0.002044882221487525839, 0.003063384235218491979, 0.004081886248949458118 ),
 .UNSPECIFIED. ) ;
#17955 = DIRECTION ( 'NONE',  ( 0.000000000000000000, -1.000000000000000000, 0.000000000000000000 ) ) ;
#17956 = PRODUCT_DEFINITION_CONTEXT ( 'detailed design', #7285, 'design' ) ;
#17957 = CARTESIAN_POINT ( 'NONE',  ( 8.134732861516145164, -38.27090915285195649, -9.000000000000000000 ) ) ;
#17958 = CARTESIAN_POINT ( 'NONE',  ( 2.682243648011666703, 3.070208061305304881, -0.04852650426601266831 ) ) ;
#17959 = CARTESIAN_POINT ( 'NONE',  ( 51.97223112728249816, 56.60051614449765367, -5.992620115222793586 ) ) ;
#17960 = DIRECTION ( 'NONE',  ( 0.000000000000000000, 0.000000000000000000, 1.000000000000000000 ) ) ;
#17961 = PLANE ( 'NONE',  #7073 ) ;
#17962 = CARTESIAN_POINT ( 'NONE',  ( 43.69122665457040000, 54.99948385550239749, 0.02388180880521036456 ) ) ;
#17963 = CARTESIAN_POINT ( 'NONE',  ( 1.257172072275274388, -3.892973519170983110, -3.433252694550781303 ) ) ;
#17964 = CARTESIAN_POINT ( 'NONE',  ( 44.03140696652192787, 51.19948385550238612, -4.306917132069425058 ) ) ;
#17965 = CARTESIAN_POINT ( 'NONE',  ( 42.38452918213190657, 55.90051614449766504, 2.450534656007115508 ) ) ;
#17966 = CARTESIAN_POINT ( 'NONE',  ( 6.506891779418575439, -5.826362946429633816, -0.09155664655282159947 ) ) ;
#17967 = CARTESIAN_POINT ( 'NONE',  ( -154.9999999999999716, -14.99999999999999645, -15.00000000000000000 ) ) ;
#17968 = ORIENTED_EDGE ( 'NONE', *, *, #11758, .F. ) ;
#17969 = CARTESIAN_POINT ( 'NONE',  ( -10.75570504584948139, -3.819660112501066518, -9.000000000000000000 ) ) ;
#17970 = SURFACE_SIDE_STYLE ('',( #4529 ) ) ;
#17971 = ADVANCED_FACE ( 'NONE', ( #11577 ), #12954, .T. ) ;
#17972 = PRODUCT_CONTEXT ( 'NONE', #18817, 'mechanical' ) ;
#17973 = ORIENTED_EDGE ( 'NONE', *, *, #18992, .T. ) ;
#17974 = DIRECTION ( 'NONE',  ( 0.000000000000000000, 0.000000000000000000, 1.000000000000000000 ) ) ;
#17975 = ADVANCED_FACE ( 'NONE', ( #16012 ), #10298, .F. ) ;
#17976 = FACE_OUTER_BOUND ( 'NONE', #9376, .T. ) ;
#17977 = CARTESIAN_POINT ( 'NONE',  ( 47.70284917648453415, 63.39948385550239607, -6.992620115222774047 ) ) ;
#17978 = DIRECTION ( 'NONE',  ( 0.000000000000000000, 0.000000000000000000, -1.000000000000000000 ) ) ;
#17979 = CARTESIAN_POINT ( 'NONE',  ( -20.00000000000000000, -19.99999999999999289, -23.00000000000000000 ) ) ;
#17980 = DIRECTION ( 'NONE',  ( 1.000000000000000000, 0.000000000000000000, 0.000000000000000000 ) ) ;
#17981 = CARTESIAN_POINT ( 'NONE',  ( 49.97728705011488159, 57.49948385550241170, -7.000000000000000888 ) ) ;
#17982 = DIRECTION ( 'NONE',  ( -1.000000000000000000, -0.000000000000000000, -0.000000000000000000 ) ) ;
#17983 = CARTESIAN_POINT ( 'NONE',  ( 43.20883090819745576, 52.79948385550240175, 4.963592699179006473 ) ) ;
#17984 = CARTESIAN_POINT ( 'NONE',  ( 3.972066048304772501, -3.435565134476469495, -1.180968096049828775 ) ) ;
#17985 = CARTESIAN_POINT ( 'NONE',  ( 54.09612160359792199, 57.30051614449765651, 5.676469297603124353 ) ) ;
#17986 = CARTESIAN_POINT ( 'NONE',  ( 4.175813232069146785, -2.061359961916366057, 3.570380186727398542 ) ) ;
#17987 = ORIENTED_EDGE ( 'NONE', *, *, #14779, .F. ) ;
#17988 = VECTOR ( 'NONE', #15542, 1000.000000000000000 ) ;
#17989 = ORIENTED_EDGE ( 'NONE', *, *, #7250, .F. ) ;
#17990 = AXIS2_PLACEMENT_3D ( 'NONE', #11483, #6981, #17492 ) ;
#17991 = FACE_BOUND ( 'NONE', #3891, .T. ) ;
#17992 = ORIENTED_EDGE ( 'NONE', *, *, #14293, .T. ) ;
#17993 = DIRECTION ( 'NONE',  ( 1.000000000000000000, 0.000000000000000000, 0.000000000000000000 ) ) ;
#17994 = CARTESIAN_POINT ( 'NONE',  ( 52.29715082351547295, 62.39948385550239607, 6.992620115222774047 ) ) ;
#17995 = VERTEX_POINT ( 'NONE', #19364 ) ;
#17996 = LINE ( 'NONE', #3190, #3058 ) ;
#17997 = VERTEX_POINT ( 'NONE', #17592 ) ;
#17998 = CARTESIAN_POINT ( 'NONE',  ( 2.449293598294706513E-15, -20.00000000000000000, 9.000000000000000000 ) ) ;
#17999 = LINE ( 'NONE', #8956, #7639 ) ;
#18000 = CARTESIAN_POINT ( 'NONE',  ( 55.11794222512601493, 56.19948385550240744, 3.688883143319541702 ) ) ;
#18001 = AXIS2_PLACEMENT_3D ( 'NONE', #8158, #10901, #14132 ) ;
#18002 = CARTESIAN_POINT ( 'NONE',  ( -154.9999999999999716, -14.99999999999999645, -6.499999999999999112 ) ) ;
#18003 = FILL_AREA_STYLE_COLOUR ( '', #12762 ) ;
#18004 = CARTESIAN_POINT ( 'NONE',  ( 56.81924384183006538, 54.80051614449764941, -4.924951120819380357 ) ) ;
#18005 = AXIS2_PLACEMENT_3D ( 'NONE', #17372, #6960, #14405 ) ;
#18006 = CARTESIAN_POINT ( 'NONE',  ( 44.91013252490150620, 58.20051614449766220, -3.727524721679154940 ) ) ;
#18007 = CARTESIAN_POINT ( 'NONE',  ( 0.1374368770859597522, -4.808326913195983821, 0.000000000000000000 ) ) ;
#18008 = CARTESIAN_POINT ( 'NONE',  ( -54.99999999999996447, -22.99999999999998579, 10.00000000000000000 ) ) ;
#18009 = ORIENTED_EDGE ( 'NONE', *, *, #15556, .F. ) ;
#18010 = ORIENTED_EDGE ( 'NONE', *, *, #3832, .F. ) ;
#18011 = DIRECTION ( 'NONE',  ( 0.000000000000000000, 0.000000000000000000, 1.000000000000000000 ) ) ;
#18012 = EDGE_LOOP ( 'NONE', ( #13193, #5408, #3369, #5339 ) ) ;
#18013 = CARTESIAN_POINT ( 'NONE',  ( 57.36023556966787851, 63.99948385550241881, -0.02388180880522424582 ) ) ;
#18014 = LINE ( 'NONE', #10532, #12468 ) ;
#18015 = ORIENTED_EDGE ( 'NONE', *, *, #15162, .F. ) ;
#18016 = VECTOR ( 'NONE', #14282, 1000.000000000000000 ) ;
#18017 = FACE_OUTER_BOUND ( 'NONE', #14963, .T. ) ;
#18018 = CARTESIAN_POINT ( 'NONE',  ( 43.34962307344081012, 46.89948385550240317, 2.184720259617164650 ) ) ;
#18019 = ORIENTED_EDGE ( 'NONE', *, *, #10957, .F. ) ;
#18020 = CYLINDRICAL_SURFACE ( 'NONE', #1932, 3.800000000000000266 ) ;
#18021 = VERTEX_POINT ( 'NONE', #7173 ) ;
#18022 = CARTESIAN_POINT ( 'NONE',  ( 43.20883090819742023, 64.20051614449766930, -4.963592699178938972 ) ) ;
#18023 = CARTESIAN_POINT ( 'NONE',  ( 53.45216259278994642, 45.00000000000002132, -5.549029329376620190 ) ) ;
#18024 = CARTESIAN_POINT ( 'NONE',  ( 42.63976443033212860, 60.99948385550238328, 0.02388180880522514787 ) ) ;
#18025 = DIRECTION ( 'NONE',  ( -1.000000000000000000, 0.000000000000000000, 0.000000000000000000 ) ) ;
#18026 = CARTESIAN_POINT ( 'NONE',  ( 4.078421086530217288, -3.990950201428958621, 0.000000000000000000 ) ) ;
#18027 = CARTESIAN_POINT ( 'NONE',  ( 56.65037692655921120, 53.10051614449766078, 2.184720259617097593 ) ) ;
#18028 = LINE ( 'NONE', #13211, #12364 ) ;
#18029 = FACE_OUTER_BOUND ( 'NONE', #11502, .T. ) ;
#18030 = ORIENTED_EDGE ( 'NONE', *, *, #4748, .T. ) ;
#18031 = EDGE_CURVE ( 'NONE', #17889, #12519, #1012, .T. ) ;
#18032 = ORIENTED_EDGE ( 'NONE', *, *, #50, .F. ) ;
#18033 = ORIENTED_EDGE ( 'NONE', *, *, #13165, .F. ) ;
#18034 = CARTESIAN_POINT ( 'NONE',  ( 4.071447262713888016, 4.041451884327382338, 0.000000000000000000 ) ) ;
#18035 = VECTOR ( 'NONE', #13444, 1000.000000000000000 ) ;
#18036 = EDGE_CURVE ( 'NONE', #10379, #13579, #10009, .T. ) ;
#18037 = CARTESIAN_POINT ( 'NONE',  ( 54.09612160359786515, 47.69948385550240744, -5.676469297603166098 ) ) ;
#18038 = SURFACE_STYLE_USAGE ( .BOTH. , #14494 ) ;
#18039 = ORIENTED_EDGE ( 'NONE', *, *, #14651, .T. ) ;
#18040 = CARTESIAN_POINT ( 'NONE',  ( 2.449293598294706513E-15, -20.00000000000000000, 9.000000000000000000 ) ) ;
#18041 = ADVANCED_FACE ( 'NONE', ( #1102 ), #2597, .F. ) ;
#18042 = ADVANCED_FACE ( 'NONE', ( #14816 ), #1396, .T. ) ;
#18043 = CIRCLE ( 'NONE', #5180, 1.000000000000000000 ) ;
#18044 = VERTEX_POINT ( 'NONE', #4145 ) ;
#18045 = CARTESIAN_POINT ( 'NONE',  ( 57.36023556966787851, 59.00051614449765935, 0.02388180880515038476 ) ) ;
#18046 = ORIENTED_EDGE ( 'NONE', *, *, #10467, .T. ) ;
#18047 = EDGE_CURVE ( 'NONE', #3558, #17750, #5950, .T. ) ;
#18048 = DIRECTION ( 'NONE',  ( 0.000000000000000000, 0.000000000000000000, 1.000000000000000000 ) ) ;
#18049 = DIRECTION ( 'NONE',  ( 0.000000000000000000, 0.000000000000000000, -1.000000000000000000 ) ) ;
#18050 = CARTESIAN_POINT ( 'NONE',  ( 46.49166364869456913, 52.30051614449766362, -4.867452303228181343 ) ) ;
#18051 = CARTESIAN_POINT ( 'NONE',  ( 5.599999999999998757, 0.000000000000000000, 0.000000000000000000 ) ) ;
#18052 = VECTOR ( 'NONE', #2253, 1000.000000000000000 ) ;
#18053 = CARTESIAN_POINT ( 'NONE',  ( 2.449293598294706513E-15, -20.00000000000000000, -8.999999999999998224 ) ) ;
#18054 = CARTESIAN_POINT ( 'NONE',  ( 48.07319477248768180, 56.59948385550239891, 6.007379884777225953 ) ) ;
#18055 = DIRECTION ( 'NONE',  ( 1.000000000000000000, 0.000000000000000000, 0.000000000000000000 ) ) ;
#18056 = ADVANCED_FACE ( 'NONE', ( #8739 ), #10196, .F. ) ;
#18057 = CARTESIAN_POINT ( 'NONE',  ( 54.72065718078918906, 54.70051614449765509, -6.458785618021089192 ) ) ;
#18058 = CARTESIAN_POINT ( 'NONE',  ( -4.000000000000000000, -2.309401076758515803, -0.4999999999999995559 ) ) ;
#18059 = CARTESIAN_POINT ( 'NONE',  ( 4.180345304246196214, 2.049116244671343345, -3.591763845239305919 ) ) ;
#18060 = PRESENTATION_LAYER_ASSIGNMENT (  '', '', ( #15529 ) ) ;
#18061 = EDGE_CURVE ( 'NONE', #950, #2819, #9453, .T. ) ;
#18062 = EDGE_LOOP ( 'NONE', ( #17816, #3287, #15152, #14078 ) ) ;
#18063 = CARTESIAN_POINT ( 'NONE',  ( 1.599999999999999867, -5.408326913195983465, -0.8000000000000000444 ) ) ;
#18064 = SURFACE_STYLE_FILL_AREA ( #12344 ) ;
#18065 = ITEM_DEFINED_TRANSFORMATION ( 'NONE', 'NONE', #11865,  #10359 ) ;
#18066 = ORIENTED_EDGE ( 'NONE', *, *, #13692, .T. ) ;
#18067 = DIRECTION ( 'NONE',  ( 0.000000000000000000, 0.000000000000000000, 1.000000000000000000 ) ) ;
#18068 = DIRECTION ( 'NONE',  ( -0.3090169943749382919, -0.9510565162951566398, 0.000000000000000000 ) ) ;
#18069 =( REPRESENTATION_RELATIONSHIP ('NONE','NONE', #16703, #4676 ) REPRESENTATION_RELATIONSHIP_WITH_TRANSFORMATION ( #18065 )SHAPE_REPRESENTATION_RELATIONSHIP( ) );
#18070 = CARTESIAN_POINT ( 'NONE',  ( 44.03140696652193498, 65.19948385550240744, -4.306917132069424170 ) ) ;
#18071 = DIRECTION ( 'NONE',  ( 1.000000000000000000, 0.000000000000000000, 0.000000000000000000 ) ) ;
#18072 = CARTESIAN_POINT ( 'NONE',  ( -0.9999999999999995559, -15.10102051443364246, -8.999999999999998224 ) ) ;
#18073 = CARTESIAN_POINT ( 'NONE',  ( -9.999999999999998224, 15.00000000000001776, 9.999999999999998224 ) ) ;
#18074 = CARTESIAN_POINT ( 'NONE',  ( 44.03140696652192787, 57.19948385550238612, -4.306917132069425058 ) ) ;
#18075 = DIRECTION ( 'NONE',  ( 0.9396926207859138680, 1.150791560227856926E-16, -0.3420201433256536139 ) ) ;
#18076 = VECTOR ( 'NONE', #16426, 1000.000000000000114 ) ;
#18077 = CARTESIAN_POINT ( 'NONE',  ( 45.31609314410967926, 50.69948385550240744, 6.485486291978119766 ) ) ;
#18078 = FACE_BOUND ( 'NONE', #12714, .T. ) ;
#18079 = CARTESIAN_POINT ( 'NONE',  ( 54.09612160359792199, 53.30051614449766362, 5.676469297603124353 ) ) ;
#18080 = EDGE_CURVE ( 'NONE', #5970, #730, #10939, .T. ) ;
#18081 = SHAPE_REPRESENTATION ( 'angular contact ball bearing_68_iso_ISO 15 ABB - 178 - 20,SI,NC,20_68', ( #10359 ), #1557 ) ;
#18082 = CARTESIAN_POINT ( 'NONE',  ( 2.449293598294706513E-15, -20.00000000000000000, 9.000000000000000000 ) ) ;
#18083 = ORIENTED_EDGE ( 'NONE', *, *, #11304, .T. ) ;
#18084 = CLOSED_SHELL ( 'NONE', ( #13482, #6744, #3461, #2706, #6169, #7264 ) ) ;
#18085 = EDGE_CURVE ( 'NONE', #15181, #18720, #11755, .T. ) ;
#18086 = VERTEX_POINT ( 'NONE', #1293 ) ;
#18087 = CIRCLE ( 'NONE', #5857, 4.000000000000000000 ) ;
#18088 = CARTESIAN_POINT ( 'NONE',  ( 75.00000000000001421, -7.499999999999971578, -10.00000000000000000 ) ) ;
#18089 = VECTOR ( 'NONE', #6647, 1000.000000000000000 ) ;
#18090 = ORIENTED_EDGE ( 'NONE', *, *, #11403, .F. ) ;
#18091 = CARTESIAN_POINT ( 'NONE',  ( 7.211304515372821022, -38.65468003441933575, -9.000000000000000000 ) ) ;
#18092 = CARTESIAN_POINT ( 'NONE',  ( 47.74827507625478518, 62.59948385550240602, 7.007379884777227730 ) ) ;
#18093 = DIRECTION ( 'NONE',  ( 0.000000000000000000, 0.000000000000000000, 1.000000000000000000 ) ) ;
#18094 = ORIENTED_EDGE ( 'NONE', *, *, #15282, .T. ) ;
#18095 = CARTESIAN_POINT ( 'NONE',  ( -149.0000000000000000, -14.99999999999999645, -6.499999999999999112 ) ) ;
#18096 = PLANE ( 'NONE',  #15458 ) ;
#18097 = EDGE_CURVE ( 'NONE', #17070, #17340, #9999, .T. ) ;
#18098 = CARTESIAN_POINT ( 'NONE',  ( 53.50833635130540955, 55.69948385550240744, -4.867452303228209765 ) ) ;
#18099 = DIRECTION ( 'NONE',  ( 1.000000000000000000, 0.000000000000000000, 0.000000000000000000 ) ) ;
#18100 = FACE_OUTER_BOUND ( 'NONE', #7342, .T. ) ;
#18101 = CARTESIAN_POINT ( 'NONE',  ( 41.58830220609386430, 52.00051614449766646, -0.02388180880514929535 ) ) ;
#18102 = EDGE_CURVE ( 'NONE', #16158, #15972, #5699, .T. ) ;
#18103 = CARTESIAN_POINT ( 'NONE',  ( 51.97223112728249816, 52.60051614449765367, -5.992620115222793586 ) ) ;
#18104 = CIRCLE ( 'NONE', #15252, 3.799999999999993605 ) ;
#18105 = CARTESIAN_POINT ( 'NONE',  ( 62.49999999999998579, 5.000000000000018652, -5.000000000000000000 ) ) ;
#18106 = CIRCLE ( 'NONE', #9612, 15.00000000000000000 ) ;
#18107 = DIRECTION ( 'NONE',  ( 0.000000000000000000, 0.000000000000000000, -1.000000000000000000 ) ) ;
#18108 = ORIENTED_EDGE ( 'NONE', *, *, #17924, .T. ) ;
#18109 = ORIENTED_EDGE ( 'NONE', *, *, #5919, .F. ) ;
#18110 = DIRECTION ( 'NONE',  ( 0.000000000000000000, 0.000000000000000000, 1.000000000000000000 ) ) ;
#18111 = EDGE_LOOP ( 'NONE', ( #1660, #2800 ) ) ;
#18112 = CARTESIAN_POINT ( 'NONE',  ( 55.96859303347804371, 64.19948385550239323, 4.306917132069425946 ) ) ;
#18113 = CARTESIAN_POINT ( 'NONE',  ( 0.1999999999999987899, 0.000000000000000000, 3.299999999999999822 ) ) ;
#18114 = AXIS2_PLACEMENT_3D ( 'NONE', #6689, #12672, #3562 ) ;
#18115 = VERTEX_POINT ( 'NONE', #10392 ) ;
#18116 = DIRECTION ( 'NONE',  ( 0.000000000000000000, 0.000000000000000000, -1.000000000000000000 ) ) ;
#18117 = CARTESIAN_POINT ( 'NONE',  ( 54.13287192849676188, 46.29948385550240886, 5.649768623646098220 ) ) ;
#18118 = CIRCLE ( 'NONE', #3378, 20.00000000000000000 ) ;
#18119 = ORIENTED_EDGE ( 'NONE', *, *, #5991, .F. ) ;
#18120 = LINE ( 'NONE', #13499, #13813 ) ;
#18121 = ORIENTED_EDGE ( 'NONE', *, *, #5852, .T. ) ;
#18122 = CARTESIAN_POINT ( 'NONE',  ( 54.68390685589039890, 63.30051614449767072, 6.485486291978072693 ) ) ;
#18123 = DIRECTION ( 'NONE',  ( 1.000000000000000000, 0.000000000000000000, 0.000000000000000000 ) ) ;
#18124 = CARTESIAN_POINT ( 'NONE',  ( 54.09612160359786515, 57.69948385550240744, -5.676469297603166098 ) ) ;
#18125 = CARTESIAN_POINT ( 'NONE',  ( 1.000000000000000000, -4.808326913195983821, -0.8000000000000000444 ) ) ;
#18126 =( NAMED_UNIT ( * ) PLANE_ANGLE_UNIT ( ) SI_UNIT ( $, .RADIAN. ) );
#18127 = CARTESIAN_POINT ( 'NONE',  ( 56.66441430157294690, 54.90051614449765793, -2.141517661632166281 ) ) ;
#18128 = CARTESIAN_POINT ( 'NONE',  ( 4.175813232069148562, -2.061359961916374051, -3.570380186727397653 ) ) ;
#18129 = CARTESIAN_POINT ( 'NONE',  ( 10.93224627749321876, -36.74771600333119181, 0.000000000000000000 ) ) ;
#18130 = B_SPLINE_CURVE_WITH_KNOTS ( 'NONE', 3,
 ( #18058, #9559, #7646, #6181, #3692, #12152 ),
 .UNSPECIFIED., .F., .F.,
 ( 4, 2, 4 ),
 ( 0.003358874760055550156, 0.004541967308452096383, 0.005725059856848641743 ),
 .UNSPECIFIED. ) ;
#18131 = CYLINDRICAL_SURFACE ( 'NONE', #15368, 0.9999999999999991118 ) ;
#18132 = EDGE_LOOP ( 'NONE', ( #11596, #17240, #7432 ) ) ;
#18133=STYLED_ITEM('',(#19468),#14979);
#18134 = VECTOR ( 'NONE', #5471, 1000.000000000000000 ) ;
#18135 = ORIENTED_EDGE ( 'NONE', *, *, #9498, .F. ) ;
#18136 = EDGE_LOOP ( 'NONE', ( #10035, #1558, #12886, #4509, #3233, #11214, #16946 ) ) ;
#18137 = DIRECTION ( 'NONE',  ( 1.000000000000000000, 0.000000000000000000, 0.000000000000000000 ) ) ;
#18138 = CARTESIAN_POINT ( 'NONE',  ( 47.74827507625478518, 46.59948385550239891, 7.007379884777227730 ) ) ;
#18139 = CARTESIAN_POINT ( 'NONE',  ( 0.1481481481481481122, -4.797713218419819903, -1.000000000000000000 ) ) ;
#18140 = VERTEX_POINT ( 'NONE', #7266 ) ;
#18141 = CARTESIAN_POINT ( 'NONE',  ( 22.00000000000000000, -20.00000000000000000, -20.00000000000000000 ) ) ;
#18142 = VERTEX_POINT ( 'NONE', #14603 ) ;
#18143 = CARTESIAN_POINT ( 'NONE',  ( 54.13287192849671214, 58.70051614449765509, -5.649768623646139964 ) ) ;
#18144 = ORIENTED_EDGE ( 'NONE', *, *, #5937, .T. ) ;
#18145 = EDGE_CURVE ( 'NONE', #6664, #8664, #6884, .T. ) ;
#18146 = AXIS2_PLACEMENT_3D ( 'NONE', #1663, #18523, #5066 ) ;
#18147 = CARTESIAN_POINT ( 'NONE',  ( 0.1085714285714285687, -3.798448662927795372, -0.8000000000000000444 ) ) ;
#18148 = UNCERTAINTY_MEASURE_WITH_UNIT (LENGTH_MEASURE( 1.000000000000000082E-05 ), #18375, 'distance_accuracy_value', 'NONE');
#18149 = DIRECTION ( 'NONE',  ( -9.710251638871371392E-17, -5.969973981896233748E-17, -1.000000000000000000 ) ) ;
#18150 = CARTESIAN_POINT ( 'NONE',  ( 55.71335778527780036, 52.90051614449766504, -1.832500667257213056 ) ) ;
#18151 = CARTESIAN_POINT ( 'NONE',  ( 75.00000000000002842, -39.99999999999998579, 10.00000000000000000 ) ) ;
#18152 = CARTESIAN_POINT ( 'NONE',  ( -18.00000000000000355, -19.99999999999999289, -20.00000000000000000 ) ) ;
#18153 = CARTESIAN_POINT ( 'NONE',  ( 53.54508667620428497, 58.29948385550240886, 4.840751629271157874 ) ) ;
#18154 = STYLED_ITEM ( 'NONE', ( #11519 ), #1480 ) ;
#18155 = CARTESIAN_POINT ( 'NONE',  ( -20.63749999999999574, 0.000000000000000000, -6.000000000000001776 ) ) ;
#18156 = CARTESIAN_POINT ( 'NONE',  ( 56.81924384183006538, 54.80051614449764941, -4.924951120819380357 ) ) ;
#18157 = EDGE_CURVE ( 'NONE', #762, #10511, #15534, .T. ) ;
#18158 = CARTESIAN_POINT ( 'NONE',  ( -9.999999999999996447, 0.000000000000000000, -9.999999999999998224 ) ) ;
#18159 = CARTESIAN_POINT ( 'NONE',  ( 4.071447262713887127, -2.020725942163686284, 3.500000000000000444 ) ) ;
#18160 = ORIENTED_EDGE ( 'NONE', *, *, #10836, .T. ) ;
#18161 = CARTESIAN_POINT ( 'NONE',  ( 2.449293598294706513E-15, -20.00000000000000000, 9.000000000000000000 ) ) ;
#18162 = VECTOR ( 'NONE', #16824, 1000.000000000000000 ) ;
#18163 = VECTOR ( 'NONE', #16124, 1000.000000000000000 ) ;
#18164 = EDGE_CURVE ( 'NONE', #17065, #8420, #5891, .T. ) ;
#18165 = ADVANCED_FACE ( 'NONE', ( #16294 ), #13044, .F. ) ;
#18166 = ORIENTED_EDGE ( 'NONE', *, *, #9480, .F. ) ;
#18167 = CARTESIAN_POINT ( 'NONE',  ( -19.89043790736547379, -17.90943073464699609, 9.000000000000000000 ) ) ;
#18168 = CARTESIAN_POINT ( 'NONE',  ( 3.973514160553462737, 3.435084588004190476, -1.181876024140317227 ) ) ;
#18169 = CIRCLE ( 'NONE', #9678, 4.799999999999999822 ) ;
#18170 = B_SPLINE_CURVE_WITH_KNOTS ( 'NONE', 3,
 ( #10567, #10669, #17853, #6170, #3238, #9198, #4514, #9005 ),
 .UNSPECIFIED., .F., .F.,
 ( 4, 2, 2, 4 ),
 ( 0.000000000000000000, 0.001493104274552342322, 0.002986208549104684210, 0.005972417098209366684 ),
 .UNSPECIFIED. ) ;
#18171 = EDGE_CURVE ( 'NONE', #17145, #950, #18371, .T. ) ;
#18172 = CARTESIAN_POINT ( 'NONE',  ( 44.03140696652193498, 61.19948385550240033, -4.306917132069424170 ) ) ;
#18173 = ADVANCED_FACE ( 'NONE', ( #13436 ), #5494, .F. ) ;
#18174 = DIRECTION ( 'NONE',  ( 0.000000000000000000, 0.000000000000000000, 1.000000000000000000 ) ) ;
#18175 = CIRCLE ( 'NONE', #5624, 5.000000000000000888 ) ;
#18176 = DIRECTION ( 'NONE',  ( 0.000000000000000000, 0.000000000000000000, -1.000000000000000000 ) ) ;
#18177 = DIRECTION ( 'NONE',  ( 0.000000000000000000, 0.000000000000000000, 1.000000000000000000 ) ) ;
#18178 = CARTESIAN_POINT ( 'NONE',  ( 44.05948171654949874, 56.79948385550240886, 4.345558710429105354 ) ) ;
#18179 = CARTESIAN_POINT ( 'NONE',  ( 20.00000000000000000, -25.00000000000000711, -23.00000000000000000 ) ) ;
#18180 = CARTESIAN_POINT ( 'NONE',  ( 57.61547081786812896, 52.09948385550241312, 2.450534656007040901 ) ) ;
#18181 = FACE_OUTER_BOUND ( 'NONE', #10865, .T. ) ;
#18182 = CARTESIAN_POINT ( 'NONE',  ( 57.36023556966787851, 55.00051614449765225, 0.02388180880515038476 ) ) ;
#18183 = ADVANCED_FACE ( 'NONE', ( #17580 ), #18710, .F. ) ;
#18184 = AXIS2_PLACEMENT_3D ( 'NONE', #2104, #9343, #13763 ) ;
#18185 = EDGE_CURVE ( 'NONE', #11260, #4647, #14072, .T. ) ;
#18186 = DIRECTION ( 'NONE',  ( 0.000000000000000000, -0.000000000000000000, -1.000000000000000000 ) ) ;
#18187 = EDGE_CURVE ( 'NONE', #8385, #2130, #10310, .T. ) ;
#18188 = VERTEX_POINT ( 'NONE', #17133 ) ;
#18189 = AXIS2_PLACEMENT_3D ( 'NONE', #1689, #18264, #13635 ) ;
#18190 = CARTESIAN_POINT ( 'NONE',  ( 20.00000000000000000, -20.00000000000000000, -10.79827876554711530 ) ) ;
#18191 = AXIS2_PLACEMENT_3D ( 'NONE', #14775, #2746, #15079 ) ;
#18192 = VECTOR ( 'NONE', #13201, 999.9999999999998863 ) ;
#18193 = CARTESIAN_POINT ( 'NONE',  ( 52.25172492374528588, 49.40051614449766504, 7.007379884777204637 ) ) ;
#18194 = CARTESIAN_POINT ( 'NONE',  ( 57.36023556966787851, 63.99948385550241881, -0.02388180880522424582 ) ) ;
#18195 = AXIS2_PLACEMENT_3D ( 'NONE', #7864, #223, #12079 ) ;
#18196 = DIRECTION ( 'NONE',  ( 2.191393683118470056E-17, 7.538405132783724027E-17, 1.000000000000000000 ) ) ;
#18197 = ORIENTED_EDGE ( 'NONE', *, *, #9258, .F. ) ;
#18198 = LINE ( 'NONE', #7492, #2414 ) ;
#18199 = CARTESIAN_POINT ( 'NONE',  ( -0.1374368770859597522, -4.808326913195983821, -0.8000000000000000444 ) ) ;
#18200 = CARTESIAN_POINT ( 'NONE',  ( 44.91013252490152752, 62.79948385550240175, 3.727524721679198461 ) ) ;
#18201 = CARTESIAN_POINT ( 'NONE',  ( -155.0777214229742071, -18.79920509849242549, 15.79999999999999893 ) ) ;
#18202 = DIRECTION ( 'NONE',  ( -1.000000000000000000, 0.000000000000000000, 0.000000000000000000 ) ) ;
#18203 = CARTESIAN_POINT ( 'NONE',  ( 41.58830220609386430, 56.00051614449765935, -0.02388180880514929535 ) ) ;
#18204 = CIRCLE ( 'NONE', #8163, 4.000000000000000000 ) ;
#18205 = CARTESIAN_POINT ( 'NONE',  ( 55.08986747509849380, 53.20051614449766220, 3.727524721679155384 ) ) ;
#18207 = AXIS2_PLACEMENT_3D ( 'NONE', #16461, #7526, #10549 ) ;
#18206 = DIRECTION ( 'NONE',  ( 0.000000000000000000, 0.000000000000000000, -1.000000000000000000 ) ) ;
#18208 = VECTOR ( 'NONE', #3187, 1000.000000000000000 ) ;
#18209 = CARTESIAN_POINT ( 'NONE',  ( 1.925929944387235853E-31, 15.00000000000001599, 15.00000000000000000 ) ) ;
#18210 = ORIENTED_EDGE ( 'NONE', *, *, #6811, .T. ) ;
#18211 = ORIENTED_EDGE ( 'NONE', *, *, #1416, .T. ) ;
#18212 = FACE_OUTER_BOUND ( 'NONE', #4067, .T. ) ;
#18213 = ORIENTED_EDGE ( 'NONE', *, *, #14897, .F. ) ;
#18214 = EDGE_CURVE ( 'NONE', #4891, #4202, #1581, .T. ) ;
#18215 = LINE ( 'NONE', #7978, #16904 ) ;
#18216 = ORIENTED_EDGE ( 'NONE', *, *, #2156, .F. ) ;
#18217 = DIRECTION ( 'NONE',  ( -1.000000000000000000, -1.040834085586084257E-16, 0.000000000000000000 ) ) ;
#18218 = AXIS2_PLACEMENT_3D ( 'NONE', #15376, #1957, #12426 ) ;
#18219 = EDGE_CURVE ( 'NONE', #18786, #4901, #6563, .T. ) ;
#18220 = CARTESIAN_POINT ( 'NONE',  ( 43.34962307344081012, 52.89948385550240317, 2.184720259617164650 ) ) ;
#18221 = ORIENTED_EDGE ( 'NONE', *, *, #19127, .T. ) ;
#18222 = DIRECTION ( 'NONE',  ( -0.000000000000000000, -0.000000000000000000, 1.000000000000000000 ) ) ;
#18223 = AXIS2_PLACEMENT_3D ( 'NONE', #14376, #11723, #14668 ) ;
#18224 = EDGE_LOOP ( 'NONE', ( #11201, #528, #16279, #12042, #3040 ) ) ;
#18225 = CARTESIAN_POINT ( 'NONE',  ( 41.58830220609386430, 48.99948385550241170, 0.02388180880523263147 ) ) ;
#18226 = CIRCLE ( 'NONE', #10355, 0.9999999999999982236 ) ;
#18227 = DIRECTION ( 'NONE',  ( -1.000000000000000000, 0.000000000000000000, 0.000000000000000000 ) ) ;
#18228 = CARTESIAN_POINT ( 'NONE',  ( 42.63976443033212860, 54.99948385550241170, 0.02388180880522514787 ) ) ;
#18229 = DIRECTION ( 'NONE',  ( 0.000000000000000000, 0.000000000000000000, -1.000000000000000000 ) ) ;
#18230 = CARTESIAN_POINT ( 'NONE',  ( 0.1481481481481481122, -4.797713218419819903, 0.000000000000000000 ) ) ;
#18231 = CARTESIAN_POINT ( 'NONE',  ( 55.96859303347802239, 54.80051614449764230, -4.306917132069484566 ) ) ;
#18232 = DIRECTION ( 'NONE',  ( 1.000000000000000000, 0.000000000000000000, 0.000000000000000000 ) ) ;
#18233 = CARTESIAN_POINT ( 'NONE',  ( 6.403457969954083673, -5.776886471390910494, 4.740078563816561288E-16 ) ) ;
#18234 = EDGE_LOOP ( 'NONE', ( #6042, #19406, #18665, #5869, #19171, #15738 ) ) ;
#18235 = VERTEX_POINT ( 'NONE', #11963 ) ;
#18236 = VERTEX_POINT ( 'NONE', #11033 ) ;
#18237 = DIRECTION ( 'NONE',  ( 0.000000000000000000, 0.000000000000000000, 1.000000000000000000 ) ) ;
#18238 = CIRCLE ( 'NONE', #9747, 1.000000000000000000 ) ;
#18239 = CARTESIAN_POINT ( 'NONE',  ( 52.25172492374522903, 53.59948385550241312, -7.007379884777225953 ) ) ;
#18240 =( GEOMETRIC_REPRESENTATION_CONTEXT ( 3 ) GLOBAL_UNCERTAINTY_ASSIGNED_CONTEXT ( ( #2069 ) ) GLOBAL_UNIT_ASSIGNED_CONTEXT ( ( #15917, #12875, #11389 ) ) REPRESENTATION_CONTEXT ( 'NONE', 'WORKASPACE' ) );
#18241 = DIRECTION ( 'NONE',  ( 1.000000000000000000, 0.000000000000000000, 0.000000000000000000 ) ) ;
#18242 = ORIENTED_EDGE ( 'NONE', *, *, #773, .T. ) ;
#18243 = CARTESIAN_POINT ( 'NONE',  ( 4.158233816355333623, -39.56295201467608535, -9.000000000000000000 ) ) ;
#18244 = ORIENTED_EDGE ( 'NONE', *, *, #18659, .F. ) ;
#18245 = CARTESIAN_POINT ( 'NONE',  ( 47.74827507625470702, 62.40051614449765793, -7.007379884777204637 ) ) ;
#18246 = ORIENTED_EDGE ( 'NONE', *, *, #347, .F. ) ;
#18247 = CARTESIAN_POINT ( 'NONE',  ( -2.595115354961444076, -7.673029147243174641, -1.000000000000000000 ) ) ;
#18248 = DIRECTION ( 'NONE',  ( -1.000000000000000000, 0.000000000000000000, 0.000000000000000000 ) ) ;
#18249 = CARTESIAN_POINT ( 'NONE',  ( 55.71335778527780036, 54.90051614449765793, -1.832500667257213056 ) ) ;
#18250 = CARTESIAN_POINT ( 'NONE',  ( -19.30627432446647163, -14.77814480204146363, 0.000000000000000000 ) ) ;
#18251 = LINE ( 'NONE', #1866, #2061 ) ;
#18252 = CARTESIAN_POINT ( 'NONE',  ( 46.49166364869460466, 64.69948385550240744, 4.867452303228209765 ) ) ;
#18253 = CARTESIAN_POINT ( 'NONE',  ( 0.000000000000000000, 0.000000000000000000, -3.499999999999999556 ) ) ;
#18254 = CARTESIAN_POINT ( 'NONE',  ( 45.31609314410960820, 56.30051614449766362, -6.485486291978072693 ) ) ;
#18255 = EDGE_LOOP ( 'NONE', ( #3318, #4309, #4503, #11845, #15627, #14298, #7442 ) ) ;
#18256 = DIRECTION ( 'NONE',  ( 1.000000000000000000, 1.040834085586084257E-16, 0.000000000000000000 ) ) ;
#18257 = EDGE_CURVE ( 'NONE', #13102, #7188, #11571, .T. ) ;
#18258 = ORIENTED_EDGE ( 'NONE', *, *, #13241, .F. ) ;
#18259 = DIRECTION ( 'NONE',  ( -1.000000000000000000, -0.000000000000000000, -0.000000000000000000 ) ) ;
#18260 = CONTEXT_DEPENDENT_SHAPE_REPRESENTATION ( #7253, #9903 ) ;
#18261 = VECTOR ( 'NONE', #13135, 1000.000000000000000 ) ;
#18262 = ORIENTED_EDGE ( 'NONE', *, *, #14292, .T. ) ;
#18263 = DIRECTION ( 'NONE',  ( 0.01780247661957949992, 0.9998415233556812165, -7.576222706442768103E-17 ) ) ;
#18264 = DIRECTION ( 'NONE',  ( 1.000000000000000000, 0.000000000000000000, 0.000000000000000000 ) ) ;
#18265 = CARTESIAN_POINT ( 'NONE',  ( 57.36023556966787851, 63.99948385550241170, -0.02388180880522424582 ) ) ;
#18266 = LINE ( 'NONE', #1979, #15185 ) ;
#18267 = CARTESIAN_POINT ( 'NONE',  ( 17.85000000000000142, -20.00000000000000000, -23.00000000000000000 ) ) ;
#18268 = CARTESIAN_POINT ( 'NONE',  ( 0.8816464618332836567, -24.71833652004169934, 9.999999999999998224 ) ) ;
#18269 = CARTESIAN_POINT ( 'NONE',  ( 47.70284917648453415, 55.39948385550238896, -6.992620115222774047 ) ) ;
#18270 = EDGE_CURVE ( 'NONE', #18339, #17828, #11535, .T. ) ;
#18271 = DIRECTION ( 'NONE',  ( -1.000000000000000000, 0.000000000000000000, 0.000000000000000000 ) ) ;
#18272 = CARTESIAN_POINT ( 'NONE',  ( 47.37792948025162332, 61.39948385550240317, -7.992620115222770494 ) ) ;
#18273 = CARTESIAN_POINT ( 'NONE',  ( 55.94051828345053679, 55.20051614449766930, 4.345558710429044069 ) ) ;
#18274 = AXIS2_PLACEMENT_3D ( 'NONE', #11967, #17870, #12062 ) ;
#18275 = CARTESIAN_POINT ( 'NONE',  ( 0.1481481481481481122, -4.797713218419819903, -1.000000000000000000 ) ) ;
#18276 = DIRECTION ( 'NONE',  ( 0.000000000000000000, 0.000000000000000000, 1.000000000000000000 ) ) ;
#18277 = EDGE_CURVE ( 'NONE', #1514, #8263, #18130, .T. ) ;
#18278 = EDGE_CURVE ( 'NONE', #3771, #9070, #9656, .T. ) ;
#18279 = ORIENTED_EDGE ( 'NONE', *, *, #17457, .F. ) ;
#18280 = EDGE_CURVE ( 'NONE', #11786, #6708, #13626, .T. ) ;
#18281 = DIRECTION ( 'NONE',  ( -0.000000000000000000, -0.000000000000000000, -1.000000000000000000 ) ) ;
#18282 = CARTESIAN_POINT ( 'NONE',  ( 55.96859303347802239, 46.80051614449766362, -4.306917132069484566 ) ) ;
#18283 = EDGE_CURVE ( 'NONE', #1433, #1080, #10680, .T. ) ;
#18284 = CARTESIAN_POINT ( 'NONE',  ( 54.09612160359786515, 63.69948385550240744, -5.676469297603166098 ) ) ;
#18285 = DIRECTION ( 'NONE',  ( 0.000000000000000000, -1.000000000000000000, 0.000000000000000000 ) ) ;
#18286 = ORIENTED_EDGE ( 'NONE', *, *, #10579, .T. ) ;
#18287 = CARTESIAN_POINT ( 'NONE',  ( -154.9999999999999716, -14.99999999999999645, -15.00000000000000000 ) ) ;
#18288 = APPLICATION_CONTEXT ( 'automotive_design' ) ;
#18289 = LINE ( 'NONE', #2094, #14846 ) ;
#18290 = CARTESIAN_POINT ( 'NONE',  ( 51.97223112728249816, 44.60051614449766078, -5.992620115222793586 ) ) ;
#18291 = CARTESIAN_POINT ( 'NONE',  ( 4.000000000000000000, -2.309401076758514915, -3.433295621305383349 ) ) ;
#18292 = CARTESIAN_POINT ( 'NONE',  ( -7.211304515372564339, -38.65468003441944234, 0.000000000000000000 ) ) ;
#18293 = CARTESIAN_POINT ( 'NONE',  ( 49.97728705011495265, 59.50051614449765935, 8.000000000000001776 ) ) ;
#18294 = CARTESIAN_POINT ( 'NONE',  ( 48.02776887271750184, 57.60051614449765367, 5.992620115222795363 ) ) ;
#18295 = AXIS2_PLACEMENT_3D ( 'NONE', #9238, #1624, #16427 ) ;
#18296 = CARTESIAN_POINT ( 'NONE',  ( -62.49999999999997158, 32.50000000000001421, -9.999999999999998224 ) ) ;
#18297 = CARTESIAN_POINT ( 'NONE',  ( 6.207671477328757348, -5.338259717474211463, -0.7538629453363940858 ) ) ;
#18298 = AXIS2_PLACEMENT_3D ( 'NONE', #17200, #11096, #5034 ) ;
#18300 = ORIENTED_EDGE ( 'NONE', *, *, #19126, .T. ) ;
#18299 = ADVANCED_FACE ( 'NONE', ( #300 ), #1771, .T. ) ;
#18301 = EDGE_CURVE ( 'NONE', #8527, #13173, #13134, .T. ) ;
#18302 = VERTEX_POINT ( 'NONE', #9946 ) ;
#18303 = DIRECTION ( 'NONE',  ( 1.000000000000000000, -1.734723475976807341E-16, -0.000000000000000000 ) ) ;
#18304 = EDGE_LOOP ( 'NONE', ( #6655, #2252 ) ) ;
#18305 = DIRECTION ( 'NONE',  ( 9.858538378746663627E-23, -5.031452844637890958E-23, 1.000000000000000000 ) ) ;
#18306 = ORIENTED_EDGE ( 'NONE', *, *, #12522, .F. ) ;
#18307 = CARTESIAN_POINT ( 'NONE',  ( -54.99999999999996447, -6.999999999999985789, 15.00000000000000000 ) ) ;
#18308 = CARTESIAN_POINT ( 'NONE',  ( 50.02271294988512551, 54.49948385550240459, 7.000000000000000888 ) ) ;
#18309 = VECTOR ( 'NONE', #12375, 1000.000000000000000 ) ;
#18310 = ORIENTED_EDGE ( 'NONE', *, *, #11541, .T. ) ;
#18311 = DIRECTION ( 'NONE',  ( -1.000000000000000000, 0.000000000000000000, 0.000000000000000000 ) ) ;
#18312 = EDGE_LOOP ( 'NONE', ( #4434, #9847, #18920, #14558 ) ) ;
#18313 = CARTESIAN_POINT ( 'NONE',  ( 57.60143344285433642, 45.89948385550240317, -2.493737253992118319 ) ) ;
#18314 = VECTOR ( 'NONE', #18176, 1000.000000000000000 ) ;
#18315 = CARTESIAN_POINT ( 'NONE',  ( 4.000000000000000000, 2.309401076758515803, -0.4999999999999995559 ) ) ;
#18316 = CARTESIAN_POINT ( 'NONE',  ( 44.91013252490152752, 46.79948385550240886, 3.727524721679198461 ) ) ;
#18317 = CARTESIAN_POINT ( 'NONE',  ( -72.99999999999997158, 1.000000000000000000, -5.999999999999998224 ) ) ;
#18318 = FILL_AREA_STYLE ('',( #12407 ) ) ;
#18319 = CARTESIAN_POINT ( 'NONE',  ( 43.33558569842706021, 53.90051614449765793, 2.141517661632167169 ) ) ;
#18320 = CARTESIAN_POINT ( 'NONE',  ( -20.00000000000000000, -19.99999999999999289, -10.79827876554711530 ) ) ;
#18321 = CARTESIAN_POINT ( 'NONE',  ( 55.96859303347804371, 50.19948385550240744, 4.306917132069425946 ) ) ;
#18322 = CARTESIAN_POINT ( 'NONE',  ( 2.000000000000000000, 0.8865213383406680414, -1.535500000000000975 ) ) ;
#18323 = EDGE_CURVE ( 'NONE', #5073, #11836, #18169, .T. ) ;
#18324 = ADVANCED_FACE ( 'NONE', ( #14468 ), #8493, .T. ) ;
#18325 = VERTEX_POINT ( 'NONE', #17627 ) ;
#18326 = ORIENTED_EDGE ( 'NONE', *, *, #1106, .T. ) ;
#18327 = FACE_BOUND ( 'NONE', #14985, .T. ) ;
#18328 =( NAMED_UNIT ( * ) PLANE_ANGLE_UNIT ( ) SI_UNIT ( $, .RADIAN. ) );
#18329 = CIRCLE ( 'NONE', #158, 3.799999999999993605 ) ;
#18330 = ADVANCED_FACE ( 'NONE', ( #15945 ), #1048, .T. ) ;
#18331 = CARTESIAN_POINT ( 'NONE',  ( 47.70284917648453415, 53.39948385550238186, -6.992620115222774047 ) ) ;
#18332 = CARTESIAN_POINT ( 'NONE',  ( 4.050480423730737911, -1.376911654797406070, 3.567926555162024282 ) ) ;
#18333 = EDGE_LOOP ( 'NONE', ( #1755, #15170, #3487, #3250 ) ) ;
#18334 = DIRECTION ( 'NONE',  ( -0.000000000000000000, -0.000000000000000000, -1.000000000000000000 ) ) ;
#18335 = PRESENTATION_LAYER_ASSIGNMENT (  '', '', ( #8613 ) ) ;
#18336 = ORIENTED_EDGE ( 'NONE', *, *, #19249, .F. ) ;
#18337 = ADVANCED_BREP_SHAPE_REPRESENTATION ( '', ( #8428, #10359 ), #2171 ) ;
#18338 = CARTESIAN_POINT ( 'NONE',  ( 45.86712807150329496, 59.70051614449766220, 5.649768623646139964 ) ) ;
#18339 = VERTEX_POINT ( 'NONE', #12993 ) ;
#18340 = CARTESIAN_POINT ( 'NONE',  ( -154.9999999999999716, -14.99999999999999645, -6.499999999999999112 ) ) ;
#18341 = PRODUCT_DEFINITION_CONTEXT ( 'detailed design', #7655, 'design' ) ;
#18342 = CARTESIAN_POINT ( 'NONE',  ( -99.99999999999997158, -6.999999999999992895, -15.00000000000000000 ) ) ;
#18343 = AXIS2_PLACEMENT_3D ( 'NONE', #5290, #14401, #13035 ) ;
#18344 = AXIS2_PLACEMENT_3D ( 'NONE', #2836, #7137, #11932 ) ;
#18345 = CARTESIAN_POINT ( 'NONE',  ( 50.02271294988506156, 52.50051614449766646, -6.000000000000000888 ) ) ;
#18346 = DIRECTION ( 'NONE',  ( 0.9999419836444144449, 0.01077169184824096695, 0.000000000000000000 ) ) ;
#18347 = EDGE_CURVE ( 'NONE', #660, #18235, #313, .T. ) ;
#18348 = CARTESIAN_POINT ( 'NONE',  ( 8.134732861516145164, -38.27090915285195649, -9.000000000000000000 ) ) ;
#18349 = CYLINDRICAL_SURFACE ( 'NONE', #7837, 3.800000000000000266 ) ;
#18350 = AXIS2_PLACEMENT_3D ( 'NONE', #3829, #13907, #9790 ) ;
#18351 = CARTESIAN_POINT ( 'NONE',  ( 45.31609314410960820, 62.30051614449766362, -6.485486291978072693 ) ) ;
#18352 = EDGE_CURVE ( 'NONE', #18325, #13956, #7112, .T. ) ;
#18353 = EDGE_LOOP ( 'NONE', ( #12948, #4134, #6515, #9979 ) ) ;
#18354 = CARTESIAN_POINT ( 'NONE',  ( 73.00000000000000000, 1.000000000000000000, 6.000000000000000000 ) ) ;
#18355 = SURFACE_STYLE_USAGE ( .BOTH. , #487 ) ;
#18356 = ORIENTED_EDGE ( 'NONE', *, *, #7232, .F. ) ;
#18357 =( LENGTH_UNIT ( ) NAMED_UNIT ( * ) SI_UNIT ( .MILLI., .METRE. ) );
#18358 = ITEM_DEFINED_TRANSFORMATION ( 'NONE', 'NONE', #4682,  #10359 ) ;
#18359 = VERTEX_POINT ( 'NONE', #10051 ) ;
#18360 = FACE_OUTER_BOUND ( 'NONE', #4941, .T. ) ;
#18361 = DIRECTION ( 'NONE',  ( -1.000000000000000000, 0.000000000000000000, 0.000000000000000000 ) ) ;
#18362 = CARTESIAN_POINT ( 'NONE',  ( -74.99999999999997158, -39.99999999999998579, 10.00000000000000000 ) ) ;
#18363 = CARTESIAN_POINT ( 'NONE',  ( -8.134732861516020819, -1.729090847147989773, -9.000000000000000000 ) ) ;
#18364 = DIRECTION ( 'NONE',  ( -1.000000000000000000, 0.000000000000000000, 0.000000000000000000 ) ) ;
#18365 = DIRECTION ( 'NONE',  ( -1.000000000000000000, 0.000000000000000000, 0.000000000000000000 ) ) ;
#18366 = AXIS2_PLACEMENT_3D ( 'NONE', #970, #6840, #6651 ) ;
#18367 = CARTESIAN_POINT ( 'NONE',  ( 55.69932041026404335, 45.89948385550240317, -1.875703265242203432 ) ) ;
#18368 = CARTESIAN_POINT ( 'NONE',  ( 6.244004651191001010, 4.663678638742294602, 2.132808149174402867 ) ) ;
#18369 = CARTESIAN_POINT ( 'NONE',  ( 45.31609314410967926, 62.69948385550240744, 6.485486291978119766 ) ) ;
#18370 = CARTESIAN_POINT ( 'NONE',  ( 44.03140696652198471, 59.80051614449766362, 4.306917132069485454 ) ) ;
#18371 = B_SPLINE_CURVE_WITH_KNOTS ( 'NONE', 3,
 ( #8922, #14904, #1477, #7455 ),
 .UNSPECIFIED., .F., .F.,
 ( 4, 4 ),
 ( 2.380735200831979558E-07, 0.002921158011986727237 ),
 .UNSPECIFIED. ) ;
#18372 = DIRECTION ( 'NONE',  ( 1.000000000000000000, 0.000000000000000000, 0.000000000000000000 ) ) ;
#18373 = DIRECTION ( 'NONE',  ( -1.000000000000000000, 9.251858538542972814E-17, -0.000000000000000000 ) ) ;
#18374 = VECTOR ( 'NONE', #2734, 1000.000000000000000 ) ;
#18375 =( LENGTH_UNIT ( ) NAMED_UNIT ( * ) SI_UNIT ( .MILLI., .METRE. ) );
#18376 = ORIENTED_EDGE ( 'NONE', *, *, #18657, .T. ) ;
#18377 = CARTESIAN_POINT ( 'NONE',  ( 0.2175679805410235534, -1.691499766303381058, -3.499999999999999556 ) ) ;
#18378 = CARTESIAN_POINT ( 'NONE',  ( 50.02271294988505446, 46.50051614449765935, -7.000000000000000888 ) ) ;
#18379 = CARTESIAN_POINT ( 'NONE',  ( 43.33558569842703179, 65.09948385550239891, -2.141517661632099223 ) ) ;
#18380 = CARTESIAN_POINT ( 'NONE',  ( -44.99999999999997158, -7.499999999999971578, -10.00000000000000000 ) ) ;
#18381 = ORIENTED_EDGE ( 'NONE', *, *, #4018, .F. ) ;
#18382 = CARTESIAN_POINT ( 'NONE',  ( -154.9999999999999716, -14.99999999999999645, -3.999999999999999112 ) ) ;
#18383 = AXIS2_PLACEMENT_3D ( 'NONE', #17998, #7395, #9053 ) ;
#18384 = DIRECTION ( 'NONE',  ( 0.000000000000000000, 0.000000000000000000, 1.000000000000000000 ) ) ;
#18385 = EDGE_CURVE ( 'NONE', #12707, #11812, #18809, .T. ) ;
#18386 = CARTESIAN_POINT ( 'NONE',  ( 44.30067958973596376, 60.89948385550241028, 1.875703265242204099 ) ) ;
#18387 = FACE_OUTER_BOUND ( 'NONE', #6705, .T. ) ;
#18388 = CARTESIAN_POINT ( 'NONE',  ( 56.65037692655918988, 47.89948385550240317, -2.184720259617163762 ) ) ;
#18389 = CARTESIAN_POINT ( 'NONE',  ( 58.41169779390614281, 61.00051614449765935, 0.02388180880515032231 ) ) ;
#18390 = CARTESIAN_POINT ( 'NONE',  ( 48.02776887271750184, 53.60051614449765367, 5.992620115222795363 ) ) ;
#18391 = EDGE_CURVE ( 'NONE', #6328, #16520, #6576, .T. ) ;
#18392 = CARTESIAN_POINT ( 'NONE',  ( 2.449293598294706513E-15, -20.00000000000000000, 9.000000000000000000 ) ) ;
#18393 = CARTESIAN_POINT ( 'NONE',  ( 6.095473853218072335, -3.806361898857768544, -3.407187799184005161 ) ) ;
#18394 = ORIENTED_EDGE ( 'NONE', *, *, #19173, .T. ) ;
#18395 = EDGE_CURVE ( 'NONE', #442, #7928, #16924, .T. ) ;
#18396 = EDGE_CURVE ( 'NONE', #1857, #3727, #17871, .T. ) ;
#18397 = VECTOR ( 'NONE', #13272, 1000.000000000000000 ) ;
#18398 = ORIENTED_EDGE ( 'NONE', *, *, #3289, .F. ) ;
#18399 = DIRECTION ( 'NONE',  ( 0.000000000000000000, 0.000000000000000000, -1.000000000000000000 ) ) ;
#18400 = AXIS2_PLACEMENT_3D ( 'NONE', #9870, #15865, #2447 ) ;
#18401 = ORIENTED_EDGE ( 'NONE', *, *, #10396, .T. ) ;
#18402 = EDGE_CURVE ( 'NONE', #6795, #1052, #17424, .T. ) ;
#18403 = CARTESIAN_POINT ( 'NONE',  ( 4.175813232069146785, -2.061359961916366057, 3.570380186727398542 ) ) ;
#18404 = ORIENTED_EDGE ( 'NONE', *, *, #1991, .F. ) ;
#18405 = DIRECTION ( 'NONE',  ( 1.000000000000000000, 0.000000000000000000, 0.000000000000000000 ) ) ;
#18406 = CARTESIAN_POINT ( 'NONE',  ( 45.86712807150323812, 55.29948385550240175, -5.649768623646098220 ) ) ;
#18407 = ORIENTED_EDGE ( 'NONE', *, *, #12147, .T. ) ;
#18408 = PLANE ( 'NONE',  #13513 ) ;
#18409 = ORIENTED_EDGE ( 'NONE', *, *, #813, .F. ) ;
#18410 = CARTESIAN_POINT ( 'NONE',  ( 56.81924384183011512, 54.19948385550241454, 4.924951120819313743 ) ) ;
#18411 = CARTESIAN_POINT ( 'NONE',  ( 4.055487192203242941, 1.409979666030558354, -3.568038521265956664 ) ) ;
#18412 = ADVANCED_FACE ( 'NONE', ( #1139 ), #15754, .F. ) ;
#18413 = TOROIDAL_SURFACE ( 'NONE', #1489, 4.100000000000000533, 0.1000000000000001582 ) ;
#18414 = CARTESIAN_POINT ( 'NONE',  ( 45.86712807150323812, 61.29948385550240886, -5.649768623646098220 ) ) ;
#18415 = CARTESIAN_POINT ( 'NONE',  ( 4.175813232069146785, 2.061359961916365613, -3.570380186727397653 ) ) ;
#18416 = ADVANCED_FACE ( 'NONE', ( #9846 ), #17231, .F. ) ;
#18417 = VECTOR ( 'NONE', #7032, 1000.000000000000000 ) ;
#18418 = CARTESIAN_POINT ( 'NONE',  ( 50.02271294988505446, 58.50051614449765935, -7.000000000000000888 ) ) ;
#18419 = CARTESIAN_POINT ( 'NONE',  ( 1.149999999999998135, 0.000000000000000000, -4.000000000000000000 ) ) ;
#18420 = CARTESIAN_POINT ( 'NONE',  ( 52.29715082351547295, 60.39948385550239607, 6.992620115222774047 ) ) ;
#18421 = DIRECTION ( 'NONE',  ( -1.000000000000000000, -0.000000000000000000, -0.000000000000000000 ) ) ;
#18422 = ORIENTED_EDGE ( 'NONE', *, *, #222, .T. ) ;
#18423 = AXIS2_PLACEMENT_3D ( 'NONE', #9991, #11366, #14598 ) ;
#18424 = VERTEX_POINT ( 'NONE', #19100 ) ;
#18425 = CARTESIAN_POINT ( 'NONE',  ( -3.175194142252082852, -39.74634503291706267, 0.000000000000000000 ) ) ;
#18426 = AXIS2_PLACEMENT_3D ( 'NONE', #3459, #7765, #11173 ) ;
#18427 = CARTESIAN_POINT ( 'NONE',  ( 54.13287192849676188, 50.29948385550240175, 5.649768623646098220 ) ) ;
#18428 = DIRECTION ( 'NONE',  ( -0.000000000000000000, -0.000000000000000000, -1.000000000000000000 ) ) ;
#18429 = ORIENTED_EDGE ( 'NONE', *, *, #8449, .T. ) ;
#18430 = CARTESIAN_POINT ( 'NONE',  ( 4.630153689607048761, 6.577590292450083844E-16, 5.371010071662833063 ) ) ;
#18431 = EDGE_LOOP ( 'NONE', ( #10214, #5758, #4117, #14001 ) ) ;
#18432 = LINE ( 'NONE', #15770, #11595 ) ;
#18433 = ORIENTED_EDGE ( 'NONE', *, *, #1908, .T. ) ;
#18434 = CARTESIAN_POINT ( 'NONE',  ( -19.99999999999999289, -14.99999999999998579, -20.00000000000000000 ) ) ;
#18435 = CARTESIAN_POINT ( 'NONE',  ( 2.385244779468109755E-15, -20.00000000000000000, -9.999999999999994671 ) ) ;
#18436 = CARTESIAN_POINT ( 'NONE',  ( 49.97728705011494554, 61.50051614449766646, 6.000000000000000888 ) ) ;
#18437 = FACE_BOUND ( 'NONE', #16907, .T. ) ;
#18438 = PRESENTATION_LAYER_ASSIGNMENT (  '', '', ( #1840 ) ) ;
#18439 = DIRECTION ( 'NONE',  ( 1.734723475976806848E-16, 1.000000000000000000, 0.000000000000000000 ) ) ;
#18440 = DIRECTION ( 'NONE',  ( -0.000000000000000000, -0.000000000000000000, 1.000000000000000000 ) ) ;
#18441 = APPLICATION_CONTEXT ( 'automotive_design' ) ;
#18442 = CARTESIAN_POINT ( 'NONE',  ( 47.42335538002180328, 60.40051614449765793, -8.007379884777206414 ) ) ;
#18443 =( GEOMETRIC_REPRESENTATION_CONTEXT ( 3 ) GLOBAL_UNCERTAINTY_ASSIGNED_CONTEXT ( ( #5986 ) ) GLOBAL_UNIT_ASSIGNED_CONTEXT ( ( #5282, #3825, #978 ) ) REPRESENTATION_CONTEXT ( 'NONE', 'WORKASPACE' ) );
#18444 = VERTEX_POINT ( 'NONE', #14263 ) ;
#18445 = EDGE_LOOP ( 'NONE', ( #6255, #18433, #16589, #14761 ) ) ;
#18446 = PLANE ( 'NONE',  #3392 ) ;
#18447 = DIRECTION ( 'NONE',  ( -9.710251638871371392E-17, -5.969973981896233748E-17, -1.000000000000000000 ) ) ;
#18448 = ITEM_DEFINED_TRANSFORMATION ( 'NONE', 'NONE', #6236,  #10359 ) ;
#18449 = ORIENTED_EDGE ( 'NONE', *, *, #2095, .T. ) ;
#18450 = CARTESIAN_POINT ( 'NONE',  ( 19.97007065299861139, -18.90625500492856759, -9.000000000000000000 ) ) ;
#18451 = AXIS2_PLACEMENT_3D ( 'NONE', #6928, #18914, #11429 ) ;
#18452 = EDGE_CURVE ( 'NONE', #164, #7574, #12904, .T. ) ;
#18453 = AXIS2_PLACEMENT_3D ( 'NONE', #8969, #16242, #1240 ) ;
#18454 = DIRECTION ( 'NONE',  ( -0.000000000000000000, -0.000000000000000000, -1.000000000000000000 ) ) ;
#18455 = ORIENTED_EDGE ( 'NONE', *, *, #3244, .F. ) ;
#18456 = EDGE_CURVE ( 'NONE', #11695, #9447, #2198, .T. ) ;
#18457 = CARTESIAN_POINT ( 'NONE',  ( -3.158233816355195955, -0.4370479853238878887, -9.000000000000000000 ) ) ;
#18458 = COLOUR_RGB ( '',1.000000000000000000, 0.9490196078431372140, 0.9098039215686274384 ) ;
#18459 = CARTESIAN_POINT ( 'NONE',  ( 5.599999999999999645, 0.000000000000000000, 0.000000000000000000 ) ) ;
#18460 = DIRECTION ( 'NONE',  ( 1.000000000000000000, 0.000000000000000000, 0.000000000000000000 ) ) ;
#18461 = DIRECTION ( 'NONE',  ( 0.000000000000000000, 8.673617379884036458E-16, 1.000000000000000000 ) ) ;
#18462 = CARTESIAN_POINT ( 'NONE',  ( 55.96859303347804371, 64.19948385550239323, 4.306917132069425946 ) ) ;
#18463 = DIRECTION ( 'NONE',  ( 0.000000000000000000, 0.000000000000000000, 1.000000000000000000 ) ) ;
#18464 = CARTESIAN_POINT ( 'NONE',  ( 41.58830220609386430, 60.99948385550241170, 0.02388180880523263147 ) ) ;
#18465 = AXIS2_PLACEMENT_3D ( 'NONE', #16219, #6024, #7089 ) ;
#18466 = CARTESIAN_POINT ( 'NONE',  ( 50.02271294988505446, 58.50051614449765935, -7.000000000000000888 ) ) ;
#18467 = VECTOR ( 'NONE', #13384, 1000.000000000000000 ) ;
#18468 = CARTESIAN_POINT ( 'NONE',  ( -18.89043790736545603, -22.09056926535314602, 9.000000000000000000 ) ) ;
#18469 = DIRECTION ( 'NONE',  ( 1.000000000000000000, 0.000000000000000000, 0.000000000000000000 ) ) ;
#18470 = AXIS2_PLACEMENT_3D ( 'NONE', #11275, #14511, #1095 ) ;
#18471 = VERTEX_POINT ( 'NONE', #11224 ) ;
#18472 = CARTESIAN_POINT ( 'NONE',  ( 2.449293598294706513E-15, -20.00000000000000000, -8.999999999999998224 ) ) ;
#18473 = CARTESIAN_POINT ( 'NONE',  ( 6.436591462021363341, 2.894509378375959674, -5.013437306331780086 ) ) ;
#18474 = CARTESIAN_POINT ( 'NONE',  ( 54.13287192849671214, 46.70051614449766220, -5.649768623646139964 ) ) ;
#18475 = AXIS2_PLACEMENT_3D ( 'NONE', #2161, #14098, #6459 ) ;
#18476 = CARTESIAN_POINT ( 'NONE',  ( -2.649999999999988809, 15.00000000000001599, -15.00000000000000000 ) ) ;
#18477 = DIRECTION ( 'NONE',  ( -0.000000000000000000, -0.000000000000000000, -1.000000000000000000 ) ) ;
#18478 = VERTEX_POINT ( 'NONE', #947 ) ;
#18479 = CARTESIAN_POINT ( 'NONE',  ( -154.9999999999999716, -14.99999999999999645, 15.00000000000000000 ) ) ;
#18480 = CARTESIAN_POINT ( 'NONE',  ( -4.000000000000000000, -2.309401076758512694, -5.000000000000000000 ) ) ;
#18481 = B_SPLINE_CURVE_WITH_KNOTS ( 'NONE', 3,
 ( #18519, #5061, #16048, #10050, #3982, #17132, #9759, #9655 ),
 .UNSPECIFIED., .F., .F.,
 ( 4, 2, 2, 4 ),
 ( 7.780516681398759253E-20, 0.002450665683189819696, 0.003675998524784729327, 0.004901331366379639391 ),
 .UNSPECIFIED. ) ;
#18482 = CARTESIAN_POINT ( 'NONE',  ( 48.07319477248768180, 62.59948385550238470, 6.007379884777225953 ) ) ;
#18483 = FACE_OUTER_BOUND ( 'NONE', #17565, .T. ) ;
#18484 = CARTESIAN_POINT ( 'NONE',  ( 2.449293598294706513E-15, -20.00000000000000000, 9.000000000000000000 ) ) ;
#18485 = VECTOR ( 'NONE', #17865, 1000.000000000000114 ) ;
#18486 = CARTESIAN_POINT ( 'NONE',  ( -17.32050807568879236, -10.00000000000004263, 9.000000000000000000 ) ) ;
#18487 = CARTESIAN_POINT ( 'NONE',  ( 50.02271294988505446, 60.50051614449766646, -8.000000000000001776 ) ) ;
#18488 = CARTESIAN_POINT ( 'NONE',  ( 53.54508667620424234, 60.70051614449766930, -4.840751629271188961 ) ) ;
#18489 = DIRECTION ( 'NONE',  ( -1.000000000000000000, -0.000000000000000000, -0.000000000000000000 ) ) ;
#18490 = CARTESIAN_POINT ( 'NONE',  ( 1.250000000000001110, 6.613092715395707467E-16, 5.400000000000000355 ) ) ;
#18491 = AXIS2_PLACEMENT_3D ( 'NONE', #15114, #314, #6289 ) ;
#18492 = ORIENTED_EDGE ( 'NONE', *, *, #16204, .F. ) ;
#18493 = AXIS2_PLACEMENT_3D ( 'NONE', #7318, #15153, #159 ) ;
#18494 = ORIENTED_EDGE ( 'NONE', *, *, #12268, .F. ) ;
#18495 = PLANE ( 'NONE',  #11241 ) ;
#18496 = EDGE_LOOP ( 'NONE', ( #19208, #17724, #16063, #4010 ) ) ;
#18497 = EDGE_CURVE ( 'NONE', #12683, #15949, #847, .T. ) ;
#18498 = CARTESIAN_POINT ( 'NONE',  ( 1.267864665251833278E-11, -20.00000000000000000, 9.000000000000000000 ) ) ;
#18499 = AXIS2_PLACEMENT_3D ( 'NONE', #19002, #16049, #6919 ) ;
#18500 = ORIENTED_EDGE ( 'NONE', *, *, #7036, .T. ) ;
#18501 = LINE ( 'NONE', #3389, #15033 ) ;
#18502 = CARTESIAN_POINT ( 'NONE',  ( 43.34962307344081012, 50.89948385550241028, 2.184720259617164650 ) ) ;
#18503 = ORIENTED_EDGE ( 'NONE', *, *, #18999, .F. ) ;
#18504 = CARTESIAN_POINT ( 'NONE',  ( 6.534224484704326485, -2.950930484791631780, -5.111161529262894909 ) ) ;
#18505 = ORIENTED_EDGE ( 'NONE', *, *, #7879, .T. ) ;
#18506 = CARTESIAN_POINT ( 'NONE',  ( 56.81924384183011512, 52.19948385550240744, 4.924951120819313743 ) ) ;
#18507 = CIRCLE ( 'NONE', #14420, 2.500000000000000888 ) ;
#18508 = CARTESIAN_POINT ( 'NONE',  ( 6.367873360227556567, 2.886751345948125991, 4.999999999999999112 ) ) ;
#18509 = CARTESIAN_POINT ( 'NONE',  ( 49.97728705011488159, 61.49948385550240459, -7.000000000000000888 ) ) ;
#18510 = CARTESIAN_POINT ( 'NONE',  ( 7.900000000000002132, 0.000000000000000000, 7.900000000000002132 ) ) ;
#18511 = CARTESIAN_POINT ( 'NONE',  ( 32.00000000000000000, 3.000000000000000000, 5.999999999999998224 ) ) ;
#18512 = CIRCLE ( 'NONE', #16632, 6.080745460913608902 ) ;
#18513 = AXIS2_PLACEMENT_3D ( 'NONE', #4482, #10440, #16348 ) ;
#18514 = CARTESIAN_POINT ( 'NONE',  ( 55.96859303347802239, 58.80051614449764941, -4.306917132069484566 ) ) ;
#18515 = LINE ( 'NONE', #3313, #994 ) ;
#18516 = ADVANCED_FACE ( 'NONE', ( #3984, #18907 ), #11422, .T. ) ;
#18517 = AXIS2_PLACEMENT_3D ( 'NONE', #13839, #15410, #6478 ) ;
#18518 = CARTESIAN_POINT ( 'NONE',  ( 56.65037692655918988, 55.89948385550240317, -2.184720259617163762 ) ) ;
#18519 = CARTESIAN_POINT ( 'NONE',  ( 1.411581201560190495E-15, 4.862606272033091592, -3.745885042887436622 ) ) ;
#18520 = DIRECTION ( 'NONE',  ( 4.082155997157843695E-16, -1.000000000000000000, 0.000000000000000000 ) ) ;
#18521 = VERTEX_POINT ( 'NONE', #17715 ) ;
#18522 = ORIENTED_EDGE ( 'NONE', *, *, #8208, .T. ) ;
#18523 = DIRECTION ( 'NONE',  ( 0.000000000000000000, 0.000000000000000000, 1.000000000000000000 ) ) ;
#18524 = CIRCLE ( 'NONE', #10673, 12.49999999999999645 ) ;
#18525 = ADVANCED_FACE ( 'NONE', ( #13486, #1235 ), #16436, .T. ) ;
#18526 = CARTESIAN_POINT ( 'NONE',  ( 44.03140696652192787, 49.19948385550240033, -4.306917132069425058 ) ) ;
#18527 = EDGE_CURVE ( 'NONE', #6553, #6996, #19301, .T. ) ;
#18528 = FACE_OUTER_BOUND ( 'NONE', #15297, .T. ) ;
#18529 = VECTOR ( 'NONE', #11238, 1000.000000000000114 ) ;
#18530 = ORIENTED_EDGE ( 'NONE', *, *, #12394, .T. ) ;
#18531 = AXIS2_PLACEMENT_3D ( 'NONE', #14336, #14139, #8461 ) ;
#18532 = VERTEX_POINT ( 'NONE', #6129 ) ;
#18533 = LINE ( 'NONE', #5074, #12080 ) ;
#18534 = ORIENTED_EDGE ( 'NONE', *, *, #8854, .F. ) ;
#18535 = CARTESIAN_POINT ( 'NONE',  ( 56.65037692655921120, 63.10051614449766078, 2.184720259617097593 ) ) ;
#18536 = ORIENTED_EDGE ( 'NONE', *, *, #18760, .T. ) ;
#18537 = EDGE_CURVE ( 'NONE', #8815, #8974, #11708, .T. ) ;
#18538 = CARTESIAN_POINT ( 'NONE',  ( 44.05948171654949874, 46.79948385550238754, 4.345558710429105354 ) ) ;
#18539 = PRODUCT_DEFINITION_CONTEXT ( 'detailed design', #14402, 'design' ) ;
#18540 = CARTESIAN_POINT ( 'NONE',  ( -44.99999999999997158, -40.00000000000000000, -10.00000000000000000 ) ) ;
#18541 = ADVANCED_FACE ( 'NONE', ( #61 ), #7501, .T. ) ;
#18542 = CARTESIAN_POINT ( 'NONE',  ( 44.91013252490150620, 60.20051614449766220, -3.727524721679154940 ) ) ;
#18543 = PLANE ( 'NONE',  #1729 ) ;
#18544 = EDGE_CURVE ( 'NONE', #16273, #5461, #1432, .T. ) ;
#18545 = SURFACE_STYLE_FILL_AREA ( #15573 ) ;
#18546 = LINE ( 'NONE', #15192, #16937 ) ;
#18547 = AXIS2_PLACEMENT_3D ( 'NONE', #9260, #12111, #4683 ) ;
#18548 = AXIS2_PLACEMENT_3D ( 'NONE', #12358, #10885, #701 ) ;
#18549 = CARTESIAN_POINT ( 'NONE',  ( 45.27934281921082516, 59.70051614449766220, 6.458785618021089192 ) ) ;
#18550 = VECTOR ( 'NONE', #19225, 1000.000000000000000 ) ;
#18551 = ORIENTED_EDGE ( 'NONE', *, *, #9565, .T. ) ;
#18552 = VERTEX_POINT ( 'NONE', #4667 ) ;
#18553 = DIRECTION ( 'NONE',  ( 1.000000000000000000, -0.000000000000000000, 0.000000000000000000 ) ) ;
#18554 = ADVANCED_FACE ( 'NONE', ( #19205 ), #13147, .T. ) ;
#18555 = DIRECTION ( 'NONE',  ( 1.000000000000000000, 0.000000000000000000, 0.000000000000000000 ) ) ;
#18556 = EDGE_LOOP ( 'NONE', ( #7786, #12440, #9950, #5684 ) ) ;
#18557 = CARTESIAN_POINT ( 'NONE',  ( -4.000000000000000000, -7.806255641895631925E-15, -3.142992957459232350 ) ) ;
#18558 = LINE ( 'NONE', #12642, #9078 ) ;
#18559 = VERTEX_POINT ( 'NONE', #9060 ) ;
#18560 = DIRECTION ( 'NONE',  ( -0.9135454576426043083, 0.4067366430757925477, 0.000000000000000000 ) ) ;
#18561 = AXIS2_PLACEMENT_3D ( 'NONE', #19118, #8132, #5661 ) ;
#18562 = DIRECTION ( 'NONE',  ( 0.000000000000000000, 0.000000000000000000, -1.000000000000000000 ) ) ;
#18563 = DIRECTION ( 'NONE',  ( -0.000000000000000000, -0.000000000000000000, 1.000000000000000000 ) ) ;
#18564 = CARTESIAN_POINT ( 'NONE',  ( 0.000000000000000000, 0.000000000000000000, -0.8000000000000000444 ) ) ;
#18565 = CARTESIAN_POINT ( 'NONE',  ( 52.25172492374522903, 63.59948385550237759, -7.007379884777225953 ) ) ;
#18566 = CARTESIAN_POINT ( 'NONE',  ( 8.500000000000000000, -2.886751345948119774, 4.999999999999999112 ) ) ;
#18567 = CARTESIAN_POINT ( 'NONE',  ( 41.58830220609386430, 56.99948385550241170, 0.02388180880523263147 ) ) ;
#18568 = CARTESIAN_POINT ( 'NONE',  ( 57.36023556966787851, 61.00051614449766646, 0.02388180880515038476 ) ) ;
#18569 = EDGE_CURVE ( 'NONE', #3254, #13489, #10625, .T. ) ;
#18570 = AXIS2_PLACEMENT_3D ( 'NONE', #7496, #13374, #2998 ) ;
#18571 = FACE_OUTER_BOUND ( 'NONE', #11303, .T. ) ;
#18572 = ADVANCED_FACE ( 'NONE', ( #16634, #12003, #4568 ), #17913, .T. ) ;
#18573 = FILL_AREA_STYLE ('',( #328 ) ) ;
#18574 = ORIENTED_EDGE ( 'NONE', *, *, #15988, .F. ) ;
#18575 = DIRECTION ( 'NONE',  ( 1.000000000000000000, 0.000000000000000000, 0.000000000000000000 ) ) ;
#18576 = B_SPLINE_CURVE_WITH_KNOTS ( 'NONE', 3,
 ( #8612, #4111, #12929, #8410, #14390, #18932 ),
 .UNSPECIFIED., .F., .F.,
 ( 4, 2, 4 ),
 ( 0.000000000000000000, 0.002086519881787259317, 0.004173039763574518633 ),
 .UNSPECIFIED. ) ;
#18577 = DIRECTION ( 'NONE',  ( 0.000000000000000000, -0.000000000000000000, 1.000000000000000000 ) ) ;
#18578 = CARTESIAN_POINT ( 'NONE',  ( 47.74827507625470702, 48.40051614449765793, -7.007379884777204637 ) ) ;
#18579 = CARTESIAN_POINT ( 'NONE',  ( 62.49999999999998579, 45.00000000000001421, -5.000000000000000000 ) ) ;
#18580 = DIRECTION ( 'NONE',  ( -0.000000000000000000, -0.000000000000000000, 1.000000000000000000 ) ) ;
#18581 = ORIENTED_EDGE ( 'NONE', *, *, #15751, .F. ) ;
#18582 = CARTESIAN_POINT ( 'NONE',  ( 0.4465819873852006072, 2.886751345948123770, -5.000000000000000000 ) ) ;
#18583 = CARTESIAN_POINT ( 'NONE',  ( -52.34999999999998010, -14.99999999999998579, -15.00000000000000000 ) ) ;
#18584 = CARTESIAN_POINT ( 'NONE',  ( 46.49166364869460466, 64.69948385550240744, 4.867452303228209765 ) ) ;
#18585 = CARTESIAN_POINT ( 'NONE',  ( -62.49999999999997158, 20.00000000000001421, 15.00000000000000000 ) ) ;
#18586 = CARTESIAN_POINT ( 'NONE',  ( 55.94051828345050836, 47.79948385550240886, -4.345558710429104465 ) ) ;
#18587 = CARTESIAN_POINT ( 'NONE',  ( 45.27934281921075410, 47.29948385550241596, -6.458785618021043895 ) ) ;
#18588 = CARTESIAN_POINT ( 'NONE',  ( 5.384454397937118664, 0.000000000000000000, -5.000000000000000000 ) ) ;
#18589 = CARTESIAN_POINT ( 'NONE',  ( 47.37792948025170858, 57.60051614449765367, 7.992620115222797139 ) ) ;
#18590 = CARTESIAN_POINT ( 'NONE',  ( 48.02776887271750184, 61.60051614449765367, 5.992620115222795363 ) ) ;
#18591 = EDGE_CURVE ( 'NONE', #18909, #10423, #3387, .T. ) ;
#18592 = DIRECTION ( 'NONE',  ( -0.000000000000000000, -0.000000000000000000, 1.000000000000000000 ) ) ;
#18593 = DIRECTION ( 'NONE',  ( 0.000000000000000000, 0.000000000000000000, -1.000000000000000000 ) ) ;
#18594 = ORIENTED_EDGE ( 'NONE', *, *, #18926, .F. ) ;
#18595 = EDGE_LOOP ( 'NONE', ( #8525, #986, #377, #13096 ) ) ;
#18596 = CARTESIAN_POINT ( 'NONE',  ( 5.599999999999999645, 2.020725942163686284, -3.499999999999999556 ) ) ;
#18597 = ORIENTED_EDGE ( 'NONE', *, *, #361, .F. ) ;
#18598 = CARTESIAN_POINT ( 'NONE',  ( -74.99999999999997158, -39.99999999999998579, 10.00000000000000000 ) ) ;
#18599 = ORIENTED_EDGE ( 'NONE', *, *, #14172, .F. ) ;
#18600 = CARTESIAN_POINT ( 'NONE',  ( 0.1085714285714285687, -3.798448662927795372, -0.8000000000000000444 ) ) ;
#18601 = CARTESIAN_POINT ( 'NONE',  ( 57.36023556966787851, 51.99948385550239749, -0.02388180880522424582 ) ) ;
#18602 = EDGE_LOOP ( 'NONE', ( #7047, #5685, #3384, #7625, #14044 ) ) ;
#18603 = CARTESIAN_POINT ( 'NONE',  ( 6.534533895392296010, -2.951347675328743314, -5.111884124469654900 ) ) ;
#18604 = ORIENTED_EDGE ( 'NONE', *, *, #10749, .T. ) ;
#18605 = CARTESIAN_POINT ( 'NONE',  ( 56.79116909180255135, 53.79948385550241596, -4.963592699179005585 ) ) ;
#18606 = DIRECTION ( 'NONE',  ( 0.000000000000000000, -0.000000000000000000, 1.000000000000000000 ) ) ;
#18607 = CARTESIAN_POINT ( 'NONE',  ( 43.34962307344081012, 62.89948385550241028, 2.184720259617164650 ) ) ;
#18608 = CARTESIAN_POINT ( 'NONE',  ( 3.948103430090398991, 3.379418997638670596, 1.146674596026254322 ) ) ;
#18609 = PLANE ( 'NONE',  #16217 ) ;
#18610 = CARTESIAN_POINT ( 'NONE',  ( 45.86712807150329496, 57.70051614449765509, 5.649768623646139964 ) ) ;
#18611 = CARTESIAN_POINT ( 'NONE',  ( 48.02776887271745210, 63.39948385550238896, -5.992620115222778487 ) ) ;
#18612 = CARTESIAN_POINT ( 'NONE',  ( 52.25172492374522903, 57.59948385550241312, -7.007379884777225953 ) ) ;
#18613 = CARTESIAN_POINT ( 'NONE',  ( 6.367873360227555679, -2.886751345948119774, 4.999999999999999112 ) ) ;
#18614 = CARTESIAN_POINT ( 'NONE',  ( 6.242800618755128816, -3.923709308886856206, 3.414402460854895072 ) ) ;
#18615 = ORIENTED_EDGE ( 'NONE', *, *, #15885, .F. ) ;
#18616 = B_SPLINE_CURVE_WITH_KNOTS ( 'NONE', 3,
 ( #10380, #16762, #15095, #8909, #13806, #14891, #389, #16382 ),
 .UNSPECIFIED., .F., .F.,
 ( 4, 2, 2, 4 ),
 ( 2.465131517075058656E-07, 0.001183067374689851080, 0.001774477805458923299, 0.002365888236227995517 ),
 .UNSPECIFIED. ) ;
#18617 = ORIENTED_EDGE ( 'NONE', *, *, #19024, .T. ) ;
#18618 = DIRECTION ( 'NONE',  ( -1.000000000000000000, -0.000000000000000000, -0.000000000000000000 ) ) ;
#18619 = CONICAL_SURFACE ( 'NONE', #1700, 4.000000000000000000, 0.8911886515913786111 ) ;
#18620 = CARTESIAN_POINT ( 'NONE',  ( 47.70284917648453415, 49.39948385550238896, -6.992620115222774047 ) ) ;
#18621 =( LENGTH_UNIT ( ) NAMED_UNIT ( * ) SI_UNIT ( .MILLI., .METRE. ) );
#18622 = ORIENTED_EDGE ( 'NONE', *, *, #4749, .F. ) ;
#18623 = VERTEX_POINT ( 'NONE', #7595 ) ;
#18624 = CYLINDRICAL_SURFACE ( 'NONE', #9564, 4.000000000000031086 ) ;
#18625 = ORIENTED_EDGE ( 'NONE', *, *, #13111, .T. ) ;
#18626 = CARTESIAN_POINT ( 'NONE',  ( 49.99999999999997158, 45.00000000000003553, -7.000000000000000888 ) ) ;
#18627 = EDGE_LOOP ( 'NONE', ( #16438, #4472, #12691, #15418, #16671 ) ) ;
#18628 = LINE ( 'NONE', #3425, #4744 ) ;
#18629 = CARTESIAN_POINT ( 'NONE',  ( 0.1999999999999987899, 0.000000000000000000, 0.000000000000000000 ) ) ;
#18630 = CARTESIAN_POINT ( 'NONE',  ( 55.08986747509849380, 59.20051614449766220, 3.727524721679155384 ) ) ;
#18631 = CARTESIAN_POINT ( 'NONE',  ( 1.734723475976807094E-15, 4.618802153517012954, -0.4999999999999995559 ) ) ;
#18632 = EDGE_CURVE ( 'NONE', #13823, #17116, #14649, .T. ) ;
#18633 = FACE_OUTER_BOUND ( 'NONE', #10607, .T. ) ;
#18634 = CARTESIAN_POINT ( 'NONE',  ( -154.9999999999999716, -14.99999999999999645, 15.79999999999999893 ) ) ;
#18635 = CIRCLE ( 'NONE', #4534, 5.999999999999977796 ) ;
#18636 = CARTESIAN_POINT ( 'NONE',  ( 47.37792948025170858, 59.60051614449765367, 7.992620115222797139 ) ) ;
#18637 = ADVANCED_FACE ( 'NONE', ( #10239 ), #17233, .T. ) ;
#18638 = EDGE_LOOP ( 'NONE', ( #397, #14143, #12780, #16871 ) ) ;
#18639 = ORIENTED_EDGE ( 'NONE', *, *, #17794, .T. ) ;
#18640 = CARTESIAN_POINT ( 'NONE',  ( -14.86289650954781649, -33.38261212717723936, -9.000000000000000000 ) ) ;
#18641 = ADVANCED_FACE ( 'NONE', ( #2811 ), #4370, .F. ) ;
#18642 = ADVANCED_FACE ( 'NONE', ( #2911 ), #8872, .T. ) ;
#18643 = CARTESIAN_POINT ( 'NONE',  ( 0.000000000000000000, 0.000000000000000000, 0.000000000000000000 ) ) ;
#18644 = CONTEXT_DEPENDENT_SHAPE_REPRESENTATION ( #17691, #8339 ) ;
#18645 = ORIENTED_EDGE ( 'NONE', *, *, #12280, .T. ) ;
#18646 = CARTESIAN_POINT ( 'NONE',  ( 10.00000000000000000, 15.00000000000001776, 9.999999999999998224 ) ) ;
#18647 = EDGE_CURVE ( 'NONE', #19035, #6066, #11889, .T. ) ;
#18648 = DIRECTION ( 'NONE',  ( -0.000000000000000000, 1.000000000000000000, 1.224646799147353207E-16 ) ) ;
#18649 = CIRCLE ( 'NONE', #10166, 2.649999999999988809 ) ;
#18650 = EDGE_LOOP ( 'NONE', ( #3989, #15551, #9776, #12643 ) ) ;
#18651 = CIRCLE ( 'NONE', #4546, 3.799999999999993605 ) ;
#18652 = CARTESIAN_POINT ( 'NONE',  ( -154.9999999999999716, -6.999999999999993783, 10.00000000000000000 ) ) ;
#18653 = CARTESIAN_POINT ( 'NONE',  ( 1.250000000000001110, 7.286648454926751965E-16, 5.899999999999999467 ) ) ;
#18654 = CARTESIAN_POINT ( 'NONE',  ( 4.104070371397481765, 4.047367226856738220, -5.737475420082528345E-17 ) ) ;
#18655 = CARTESIAN_POINT ( 'NONE',  ( -29.99999999999999645, -39.99999999999998579, -12.49999999999999822 ) ) ;
#18656 = AXIS2_PLACEMENT_3D ( 'NONE', #17000, #12567, #18575 ) ;
#18657 = EDGE_CURVE ( 'NONE', #8711, #2647, #3458, .T. ) ;
#18658 = DIRECTION ( 'NONE',  ( 1.000000000000000000, 0.000000000000000000, 0.000000000000000000 ) ) ;
#18659 = EDGE_CURVE ( 'NONE', #5389, #7908, #2537, .T. ) ;
#18660 = CARTESIAN_POINT ( 'NONE',  ( 43.34962307344081012, 62.89948385550241028, 2.184720259617164650 ) ) ;
#18661 = DIRECTION ( 'NONE',  ( 0.000000000000000000, 0.000000000000000000, 1.000000000000000000 ) ) ;
#18662 = CARTESIAN_POINT ( 'NONE',  ( 49.97728705011486738, 57.49948385550241170, -8.000000000000001776 ) ) ;
#18663 = CARTESIAN_POINT ( 'NONE',  ( 43.33558569842706021, 63.90051614449765793, 2.141517661632167169 ) ) ;
#18664 = CARTESIAN_POINT ( 'NONE',  ( 2.385244779468109755E-15, -20.00000000000000000, -9.999999999999994671 ) ) ;
#18665 = ORIENTED_EDGE ( 'NONE', *, *, #9615, .F. ) ;
#18666 = DIRECTION ( 'NONE',  ( -0.000000000000000000, -0.000000000000000000, 1.000000000000000000 ) ) ;
#18667 = DIRECTION ( 'NONE',  ( 1.000000000000000000, 0.000000000000000000, 0.000000000000000000 ) ) ;
#18668 = CARTESIAN_POINT ( 'NONE',  ( 54.09612160359792199, 53.30051614449766362, 5.676469297603124353 ) ) ;
#18669 = CARTESIAN_POINT ( 'NONE',  ( 4.114405500665260895, -2.025575754679711071, 3.508400121684938089 ) ) ;
#18670 = CONICAL_SURFACE ( 'NONE', #9881, 1.999999999999998224, 1.029744259999999745 ) ;
#18671 = CARTESIAN_POINT ( 'NONE',  ( 3.020236159542449172, -23.98474259401938014, -8.999999999999998224 ) ) ;
#18672 = VERTEX_POINT ( 'NONE', #12296 ) ;
#18673 = DIRECTION ( 'NONE',  ( 0.000000000000000000, 0.000000000000000000, -1.000000000000000000 ) ) ;
#18674 = LINE ( 'NONE', #5217, #7332 ) ;
#18675 = CARTESIAN_POINT ( 'NONE',  ( 17.85000000000000142, -20.00000000000000000, -23.00000000000000000 ) ) ;
#18676 = FACE_OUTER_BOUND ( 'NONE', #17089, .T. ) ;
#18677 = DIRECTION ( 'NONE',  ( 1.000000000000000000, 0.000000000000000000, 0.000000000000000000 ) ) ;
#18678 = CARTESIAN_POINT ( 'NONE',  ( 54.68390685589039890, 57.30051614449767072, 6.485486291978072693 ) ) ;
#18679 = CARTESIAN_POINT ( 'NONE',  ( 48.07319477248762496, 60.40051614449765793, -6.007379884777208190 ) ) ;
#18680 = CYLINDRICAL_SURFACE ( 'NONE', #2565, 0.5999999999999999778 ) ;
#18681 = CARTESIAN_POINT ( 'NONE',  ( 6.323290364500451233, 2.010128762267162639, 4.999999999999998224 ) ) ;
#18682 = ORIENTED_EDGE ( 'NONE', *, *, #3205, .T. ) ;
#18683 = AXIS2_PLACEMENT_3D ( 'NONE', #18053, #16387, #14898 ) ;
#18684 = ORIENTED_EDGE ( 'NONE', *, *, #17190, .F. ) ;
#18685 = EDGE_LOOP ( 'NONE', ( #11330, #8818, #18758, #10527, #11382 ) ) ;
#18686 = FACE_OUTER_BOUND ( 'NONE', #16547, .T. ) ;
#18687 = ORIENTED_EDGE ( 'NONE', *, *, #1733, .F. ) ;
#18688 = LINE ( 'NONE', #9738, #9048 ) ;
#18689 = CIRCLE ( 'NONE', #13351, 4.999999999999999112 ) ;
#18690 = VERTEX_POINT ( 'NONE', #11012 ) ;
#18691 = LINE ( 'NONE', #12689, #5659 ) ;
#18692 = CARTESIAN_POINT ( 'NONE',  ( 52.29715082351547295, 56.39948385550239607, 6.992620115222774047 ) ) ;
#18693 = ADVANCED_FACE ( 'NONE', ( #3381 ), #5131, .F. ) ;
#18694 = ORIENTED_EDGE ( 'NONE', *, *, #13710, .F. ) ;
#18695 = CARTESIAN_POINT ( 'NONE',  ( -3.175194142252069973, -39.74634503291706267, -9.000000000000000000 ) ) ;
#18696 = VERTEX_POINT ( 'NONE', #244 ) ;
#18697 = CARTESIAN_POINT ( 'NONE',  ( 49.97728705011486738, 53.49948385550240459, -8.000000000000001776 ) ) ;
#18698 = CARTESIAN_POINT ( 'NONE',  ( 3.880198502136737115, 0.7307680362927179152, -3.499999999999999556 ) ) ;
#18699 = EDGE_CURVE ( 'NONE', #5879, #17949, #3482, .T. ) ;
#18700 = CARTESIAN_POINT ( 'NONE',  ( 55.71335778527780747, 46.09948385550240602, 1.832500667257165983 ) ) ;
#18701 = CARTESIAN_POINT ( 'NONE',  ( 4.170895651974849017, 2.054890354522707074, -3.559174498016318910 ) ) ;
#18702 = CARTESIAN_POINT ( 'NONE',  ( 4.104070371397483541, -4.047367226856742661, 3.293285021600925981E-16 ) ) ;
#18703 = CARTESIAN_POINT ( 'NONE',  ( 55.94051828345053679, 61.20051614449766220, 4.345558710429044069 ) ) ;
#18704 = CARTESIAN_POINT ( 'NONE',  ( 44.88205777487398507, 63.19948385550240744, -3.688883143319540814 ) ) ;
#18705 = VECTOR ( 'NONE', #14129, 1000.000000000000000 ) ;
#18706 = CARTESIAN_POINT ( 'NONE',  ( 43.33558569842703179, 59.09948385550240602, -2.141517661632099223 ) ) ;
#18707 = CARTESIAN_POINT ( 'NONE',  ( 53.50000000000000000, 0.000000000000000000, 0.000000000000000000 ) ) ;
#18708 = CARTESIAN_POINT ( 'NONE',  ( 49.99999999999997158, 65.00000000000002842, -7.000000000000000888 ) ) ;
#18709 = ORIENTED_EDGE ( 'NONE', *, *, #15134, .T. ) ;
#18710 =( BOUNDED_SURFACE ( )  B_SPLINE_SURFACE ( 3, 2, ( 
 ( #5154, #17966, #5062 ),
 ( #15000, #3153, #12058 ),
 ( #9119, #4525, #656 ),
 ( #7742, #12, #18614 ),
 ( #10483, #15654, #16486 ),
 ( #6000, #13537, #4618 ) ),
 .UNSPECIFIED., .F., .F., .F. ) 
 B_SPLINE_SURFACE_WITH_KNOTS ( ( 4, 2, 4 ),
 ( 3, 3 ),
 ( 0.02367865728600888897, 0.02663179453327094853, 0.02958493178053300809 ),
 ( 0.000000000000000000, 1.000000000000000000 ),
 .UNSPECIFIED. ) 
 GEOMETRIC_REPRESENTATION_ITEM ( )  RATIONAL_B_SPLINE_SURFACE ( (
 ( 1.000000000000000000, 0.8047781103519399126, 1.000000000000000000),
 ( 1.000000000000000000, 0.8123785825980039954, 1.000000000000000000),
 ( 1.000000000000000000, 0.8190671539288042480, 1.000000000000000000),
 ( 1.000000000000000000, 0.8192352255335092481, 1.000000000000000000),
 ( 1.000000000000000000, 0.8126129676835893711, 1.000000000000000000),
 ( 1.000000000000000000, 0.8047712537969730073, 1.000000000000000000) ) ) 
 REPRESENTATION_ITEM ( '' )  SURFACE ( )  );
#18711 = ORIENTED_EDGE ( 'NONE', *, *, #116, .T. ) ;
#18712 = DIRECTION ( 'NONE',  ( 1.000000000000000000, 0.000000000000000000, 0.000000000000000000 ) ) ;
#18713 = ORIENTED_EDGE ( 'NONE', *, *, #18283, .F. ) ;
#18714 = CARTESIAN_POINT ( 'NONE',  ( 44.05948171654949874, 56.79948385550240886, 4.345558710429105354 ) ) ;
#18715 = DIRECTION ( 'NONE',  ( -0.000000000000000000, -0.000000000000000000, -1.000000000000000000 ) ) ;
#18716 = ORIENTED_EDGE ( 'NONE', *, *, #6518, .T. ) ;
#18717 = EDGE_LOOP ( 'NONE', ( #10398, #2571, #11234, #5357 ) ) ;
#18718 = LINE ( 'NONE', #9570, #14580 ) ;
#18719 = AXIS2_PLACEMENT_3D ( 'NONE', #12866, #14430, #13057 ) ;
#18720 = VERTEX_POINT ( 'NONE', #18490 ) ;
#18721 = CARTESIAN_POINT ( 'NONE',  ( 47.74827507625470702, 64.40051614449765793, -7.007379884777204637 ) ) ;
#18722 = EDGE_LOOP ( 'NONE', ( #15392, #12112, #16798, #14191 ) ) ;
#18723 = VECTOR ( 'NONE', #15378, 1000.000000000000000 ) ;
#18724 = CARTESIAN_POINT ( 'NONE',  ( 57.36023556966787851, 47.99948385550239038, -0.02388180880522424582 ) ) ;
#18725 = CARTESIAN_POINT ( 'NONE',  ( 0.000000000000000000, 3.031088913245533423, -1.750000000000004885 ) ) ;
#18726 = CARTESIAN_POINT ( 'NONE',  ( 56.30877334542961421, 61.00051614449765935, 0.02388180880515774693 ) ) ;
#18727 = CARTESIAN_POINT ( 'NONE',  ( 2.449293598294706513E-15, -20.00000000000000000, 9.000000000000000000 ) ) ;
#18728 = CARTESIAN_POINT ( 'NONE',  ( 0.3126073911696407026, -2.020725942163686728, 3.500000000000000444 ) ) ;
#18729 = CIRCLE ( 'NONE', #10877, 8.000000000000000000 ) ;
#18730 = ORIENTED_EDGE ( 'NONE', *, *, #2454, .T. ) ;
#18731 = ORIENTED_EDGE ( 'NONE', *, *, #16722, .T. ) ;
#18732 = CARTESIAN_POINT ( 'NONE',  ( 4.000000000000000000, -1.677850389431204459, -3.535268758346977513 ) ) ;
#18733 = VECTOR ( 'NONE', #5636, 1000.000000000000000 ) ;
#18734 = VERTEX_POINT ( 'NONE', #15336 ) ;
#18735 = CARTESIAN_POINT ( 'NONE',  ( 4.071447262713887127, 2.020725942163688504, 3.500000000000000000 ) ) ;
#18736 = ADVANCED_FACE ( 'NONE', ( #17019 ), #17336, .F. ) ;
#18737 = CYLINDRICAL_SURFACE ( 'NONE', #19132, 1.000000000000000888 ) ;
#18738 = ORIENTED_EDGE ( 'NONE', *, *, #281, .T. ) ;
#18739 = VECTOR ( 'NONE', #3373, 1000.000000000000000 ) ;
#18740 = VECTOR ( 'NONE', #15580, 1000.000000000000000 ) ;
#18741 = LINE ( 'NONE', #6566, #12856 ) ;
#18742 = LINE ( 'NONE', #1349, #17622 ) ;
#18743 = CYLINDRICAL_SURFACE ( 'NONE', #18343, 0.7499999999999997780 ) ;
#18744 = DIRECTION ( 'NONE',  ( 1.387778780781445676E-16, -1.000000000000000000, 0.000000000000000000 ) ) ;
#18745 = CARTESIAN_POINT ( 'NONE',  ( 4.071447262713887127, 2.020725942163688504, 3.500000000000000000 ) ) ;
#18746 = CARTESIAN_POINT ( 'NONE',  ( 44.28664221472220675, 47.09948385550240602, -1.832500667257165317 ) ) ;
#18747 = MECHANICAL_DESIGN_GEOMETRIC_PRESENTATION_REPRESENTATION (  '', ( #15290 ), #263 ) ;
#18748 = LINE ( 'NONE', #6858, #7563 ) ;
#18749 = CARTESIAN_POINT ( 'NONE',  ( 55.96859303347804371, 46.19948385550238612, 4.306917132069425946 ) ) ;
#18750 = CARTESIAN_POINT ( 'NONE',  ( 55.96859303347802239, 58.80051614449764941, -4.306917132069484566 ) ) ;
#18751 = EDGE_CURVE ( 'NONE', #7187, #870, #3161, .T. ) ;
#18752 = EDGE_CURVE ( 'NONE', #16440, #10629, #13471, .T. ) ;
#18753 = DIRECTION ( 'NONE',  ( -0.000000000000000000, -0.000000000000000000, -1.000000000000000000 ) ) ;
#18754 = CARTESIAN_POINT ( 'NONE',  ( 6.390820841722129941, 5.837016270311235822, 0.1100087447852453187 ) ) ;
#18755 = AXIS2_PLACEMENT_3D ( 'NONE', #14195, #9788, #778 ) ;
#18756 = AXIS2_PLACEMENT_3D ( 'NONE', #4719, #582, #4902 ) ;
#18757 = DIRECTION ( 'NONE',  ( 0.000000000000000000, 0.000000000000000000, 1.000000000000000000 ) ) ;
#18758 = ORIENTED_EDGE ( 'NONE', *, *, #5574, .T. ) ;
#18759 = DIRECTION ( 'NONE',  ( -0.000000000000000000, 0.8660254037844387076, 0.5000000000000001110 ) ) ;
#18760 = EDGE_CURVE ( 'NONE', #16254, #17767, #12197, .T. ) ;
#18761 = ADVANCED_FACE ( 'NONE', ( #10724 ), #6602, .T. ) ;
#18762 = CARTESIAN_POINT ( 'NONE',  ( 2.449293598294706513E-15, -20.00000000000000000, 9.000000000000000000 ) ) ;
#18763 = CARTESIAN_POINT ( 'NONE',  ( 52.25172492374528588, 53.40051614449765083, 7.007379884777204637 ) ) ;
#18764 = DIRECTION ( 'NONE',  ( 1.000000000000000000, 0.000000000000000000, 0.000000000000000000 ) ) ;
#18765 = CARTESIAN_POINT ( 'NONE',  ( 20.00000000000000000, -20.00000000000000000, -20.00000000000000000 ) ) ;
#18766 = ORIENTED_EDGE ( 'NONE', *, *, #12623, .T. ) ;
#18767 = FACE_OUTER_BOUND ( 'NONE', #8999, .T. ) ;
#18768 = AXIS2_PLACEMENT_3D ( 'NONE', #2821, #8784, #7509 ) ;
#18769 = PLANE ( 'NONE',  #13895 ) ;
#18770 = ADVANCED_FACE ( 'NONE', ( #10813 ), #12583, .T. ) ;
#18771 = AXIS2_PLACEMENT_3D ( 'NONE', #17042, #462, #12415 ) ;
#18772 = CARTESIAN_POINT ( 'NONE',  ( -3.098410542199071749, -7.060458129626440815, -1.000000000000000000 ) ) ;
#18773 = CARTESIAN_POINT ( 'NONE',  ( 45.90387839640214196, 48.69948385550240744, 5.676469297603166098 ) ) ;
#18774 = EDGE_CURVE ( 'NONE', #8711, #17538, #14087, .T. ) ;
#18775 = DIRECTION ( 'NONE',  ( 0.000000000000000000, 0.000000000000000000, 1.000000000000000000 ) ) ;
#18776 = CARTESIAN_POINT ( 'NONE',  ( 47.42335538002188144, 46.59948385550239891, 8.007379884777233059 ) ) ;
#18777 = CARTESIAN_POINT ( 'NONE',  ( 44.91013252490150620, 64.20051614449766930, -3.727524721679154940 ) ) ;
#18778 = EDGE_CURVE ( 'NONE', #16273, #3214, #2838, .T. ) ;
#18779 = AXIS2_PLACEMENT_3D ( 'NONE', #2288, #16003, #3845 ) ;
#18780 = DIRECTION ( 'NONE',  ( 0.000000000000000000, 1.000000000000000000, 0.000000000000000000 ) ) ;
#18781 = DIRECTION ( 'NONE',  ( -0.000000000000000000, 0.000000000000000000, -1.000000000000000000 ) ) ;
#18782 = ORIENTED_EDGE ( 'NONE', *, *, #15144, .F. ) ;
#18783 = VERTEX_POINT ( 'NONE', #14140 ) ;
#18784 = ORIENTED_EDGE ( 'NONE', *, *, #8050, .F. ) ;
#18785 = CARTESIAN_POINT ( 'NONE',  ( 4.872650870659752442, 0.4273491293402468805, 0.000000000000000000 ) ) ;
#18786 = VERTEX_POINT ( 'NONE', #5419 ) ;
#18787 = AXIS2_PLACEMENT_3D ( 'NONE', #3210, #10634, #357 ) ;
#18788 = CIRCLE ( 'NONE', #15948, 4.000000000000031086 ) ;
#18789 = CARTESIAN_POINT ( 'NONE',  ( 3.972058292797711054, 0.6948821373584146421, 3.565770528409240026 ) ) ;
#18790 = ORIENTED_EDGE ( 'NONE', *, *, #16035, .T. ) ;
#18791 = DIRECTION ( 'NONE',  ( -0.000000000000000000, -0.000000000000000000, 1.000000000000000000 ) ) ;
#18792 = CARTESIAN_POINT ( 'NONE',  ( 54.13287192849676188, 56.29948385550240175, 5.649768623646098220 ) ) ;
#18793 = EDGE_LOOP ( 'NONE', ( #8311, #19112, #9236, #19229 ) ) ;
#18794 = VECTOR ( 'NONE', #2089, 1000.000000000000000 ) ;
#18795 = CARTESIAN_POINT ( 'NONE',  ( -7.211304515372564339, -38.65468003441944234, 9.000000000000000000 ) ) ;
#18796 = ORIENTED_EDGE ( 'NONE', *, *, #15044, .F. ) ;
#18797 = CARTESIAN_POINT ( 'NONE',  ( 57.60143344285433642, 51.89948385550241028, -2.493737253992118319 ) ) ;
#18798 = CYLINDRICAL_SURFACE ( 'NONE', #14201, 1.000000000000000888 ) ;
#18799 = CARTESIAN_POINT ( 'NONE',  ( 55.08986747509847248, 51.79948385550240175, -3.727524721679197572 ) ) ;
#18800 = CARTESIAN_POINT ( 'NONE',  ( 4.158413352280813768, 2.044871626972823986, -3.541821552872968404 ) ) ;
#18801 = CARTESIAN_POINT ( 'NONE',  ( 4.151274195509681242, -4.079825909417492902, 4.401844587977598791E-16 ) ) ;
#18802 = CARTESIAN_POINT ( 'NONE',  ( 47.37792948025170858, 45.60051614449765367, 7.992620115222797139 ) ) ;
#18803 = AXIS2_PLACEMENT_3D ( 'NONE', #17770, #13340, #4231 ) ;
#18804 = CARTESIAN_POINT ( 'NONE',  ( 55.11794222512599362, 44.80051614449766362, -3.688883143319583446 ) ) ;
#18805 = CARTESIAN_POINT ( 'NONE',  ( 6.534838248920896930, -2.951765777552406878, 5.112608298763836601 ) ) ;
#18806 = CARTESIAN_POINT ( 'NONE',  ( -19.02113032590308705, -13.81966011250110249, -9.000000000000000000 ) ) ;
#18807 = VERTEX_POINT ( 'NONE', #8358 ) ;
#18808 = ADVANCED_FACE ( 'NONE', ( #8167 ), #14527, .F. ) ;
#18809 = CIRCLE ( 'NONE', #12530, 0.4999999999999972244 ) ;
#18810 = EDGE_LOOP ( 'NONE', ( #4139, #7557, #19078, #16324, #3993, #9125, #5065, #18019, #8566, #16248, #2358, #14251 ) ) ;
#18811 = DIRECTION ( 'NONE',  ( 0.000000000000000000, 0.000000000000000000, 1.000000000000000000 ) ) ;
#18812 =( NAMED_UNIT ( * ) PLANE_ANGLE_UNIT ( ) SI_UNIT ( $, .RADIAN. ) );
#18813 = ORIENTED_EDGE ( 'NONE', *, *, #11351, .T. ) ;
#18814 = ADVANCED_FACE ( 'NONE', ( #18975 ), #725, .F. ) ;
#18815 = CARTESIAN_POINT ( 'NONE',  ( 49.97728705011488159, 55.49948385550240459, -7.000000000000000888 ) ) ;
#18816 = CARTESIAN_POINT ( 'NONE',  ( -52.34999999999998010, -14.99999999999998579, 15.00000000000000178 ) ) ;
#18817 = APPLICATION_CONTEXT ( 'automotive_design' ) ;
#18818 = EDGE_LOOP ( 'NONE', ( #11451, #15629, #7341, #17209 ) ) ;
#18819 = ORIENTED_EDGE ( 'NONE', *, *, #3817, .F. ) ;
#18820 = DIRECTION ( 'NONE',  ( -0.000000000000000000, -0.000000000000000000, 1.000000000000000000 ) ) ;
#18821 = CIRCLE ( 'NONE', #18491, 2.200000000000001066 ) ;
#18822 = ORIENTED_EDGE ( 'NONE', *, *, #5122, .F. ) ;
#18823 = AXIS2_PLACEMENT_3D ( 'NONE', #5467, #11350, #8407 ) ;
#18824 = CARTESIAN_POINT ( 'NONE',  ( -31.74999999999995737, 0.000000000000000000, 3.500000000000000000 ) ) ;
#18825 = VECTOR ( 'NONE', #8880, 1000.000000000000000 ) ;
#18826 = VERTEX_POINT ( 'NONE', #5515 ) ;
#18827 = CARTESIAN_POINT ( 'NONE',  ( 45.86712807150323812, 53.29948385550240886, -5.649768623646098220 ) ) ;
#18828 = DIRECTION ( 'NONE',  ( 1.000000000000000000, 0.000000000000000000, 0.000000000000000000 ) ) ;
#18829 = VECTOR ( 'NONE', #18881, 1000.000000000000114 ) ;
#18830 = CARTESIAN_POINT ( 'NONE',  ( 55.08986747509849380, 61.20051614449766220, 3.727524721679155384 ) ) ;
#18831 = LINE ( 'NONE', #8516, #2683 ) ;
#18832 = SURFACE_STYLE_USAGE ( .BOTH. , #10073 ) ;
#18833 = CARTESIAN_POINT ( 'NONE',  ( 0.2175679805369682140, -1.691499766289324080, 3.500000000000000000 ) ) ;
#18834 = CIRCLE ( 'NONE', #16005, 4.000000000000000000 ) ;
#18835 = AXIS2_PLACEMENT_3D ( 'NONE', #4083, #14164, #3796 ) ;
#18836 = VECTOR ( 'NONE', #10997, 1000.000000000000000 ) ;
#18837 = ORIENTED_EDGE ( 'NONE', *, *, #6608, .T. ) ;
#18838 = ORIENTED_EDGE ( 'NONE', *, *, #11970, .F. ) ;
#18839 = CARTESIAN_POINT ( 'NONE',  ( 4.000000000000000000, 1.680228229147133767, -3.316631783032546021 ) ) ;
#18840 = VECTOR ( 'NONE', #7884, 1000.000000000000000 ) ;
#18841 = FACE_OUTER_BOUND ( 'NONE', #16369, .T. ) ;
#18842 = FILL_AREA_STYLE ('',( #6751 ) ) ;
#18843 = MECHANICAL_DESIGN_GEOMETRIC_PRESENTATION_REPRESENTATION (  '', ( #1921 ), #6297 ) ;
#18844 = VERTEX_POINT ( 'NONE', #11394 ) ;
#18845 = CARTESIAN_POINT ( 'NONE',  ( 6.212068001622437663, 3.310128279683251851, 4.266689640018040741 ) ) ;
#18846 = ORIENTED_EDGE ( 'NONE', *, *, #16233, .F. ) ;
#18847 = DIRECTION ( 'NONE',  ( 0.000000000000000000, 0.000000000000000000, -1.000000000000000000 ) ) ;
#18848 = CARTESIAN_POINT ( 'NONE',  ( 4.132952817037860882, 4.063368025374523462, 1.253603594387587993E-15 ) ) ;
#18849 = AXIS2_PLACEMENT_3D ( 'NONE', #10737, #18222, #16738 ) ;
#18850 = AXIS2_PLACEMENT_3D ( 'NONE', #11616, #13284, #19204 ) ;
#18851 = PLANE ( 'NONE',  #1084 ) ;
#18852 = CARTESIAN_POINT ( 'NONE',  ( 4.175075985190095373, 2.060370777630105898, 3.568666869285574972 ) ) ;
#18853 = AXIS2_PLACEMENT_3D ( 'NONE', #12963, #13163, #5720 ) ;
#18854 = CARTESIAN_POINT ( 'NONE',  ( 48.07319477248768180, 48.59948385550239891, 6.007379884777225953 ) ) ;
#18855 = DIRECTION ( 'NONE',  ( 0.9781476007338055778, 0.2079116908177597867, 0.000000000000000000 ) ) ;
#18856 = CARTESIAN_POINT ( 'NONE',  ( 42.63976443033212860, 46.99948385550240459, 0.02388180880522514787 ) ) ;
#18857 = CARTESIAN_POINT ( 'NONE',  ( 47.37792948025170858, 45.60051614449765367, 7.992620115222797139 ) ) ;
#18858 = DIRECTION ( 'NONE',  ( 1.000000000000000000, 0.000000000000000000, 0.000000000000000000 ) ) ;
#18859 = CARTESIAN_POINT ( 'NONE',  ( 6.207530437345012864, 4.849805425595251407, -1.599890596046337210 ) ) ;
#18860 = B_SPLINE_CURVE_WITH_KNOTS ( 'NONE', 3,
 ( #13405, #9270, #3223, #15168, #3504 ),
 .UNSPECIFIED., .F., .F.,
 ( 4, 1, 4 ),
 ( 0.000000000000000000, 0.002886751345948128985, 0.005773502691896257970 ),
 .UNSPECIFIED. ) ;
#18861 = DIRECTION ( 'NONE',  ( 0.000000000000000000, 0.000000000000000000, -1.000000000000000000 ) ) ;
#18862 = ORIENTED_EDGE ( 'NONE', *, *, #5927, .F. ) ;
#18863 = FILL_AREA_STYLE_COLOUR ( '', #17712 ) ;
#18864 = PRODUCT_DEFINITION_SHAPE ( 'NONE', 'NONE',  #19433 ) ;
#18865 = AXIS2_PLACEMENT_3D ( 'NONE', #14332, #916, #7183 ) ;
#18866 = CARTESIAN_POINT ( 'NONE',  ( -19.76107906696388739, -23.08216711247161967, -9.000000000000000000 ) ) ;
#18867 = CARTESIAN_POINT ( 'NONE',  ( 44.03140696652198471, 49.80051614449765651, 4.306917132069485454 ) ) ;
#18868 = DIRECTION ( 'NONE',  ( -1.000000000000000000, -3.469446951953615175E-16, -0.000000000000000000 ) ) ;
#18869 = FACE_OUTER_BOUND ( 'NONE', #12978, .T. ) ;
#18870 = ORIENTED_EDGE ( 'NONE', *, *, #8928, .F. ) ;
#18871 = CARTESIAN_POINT ( 'NONE',  ( 18.68843350152485172, -12.87662627267922666, -9.000000000000000000 ) ) ;
#18872 = FACE_BOUND ( 'NONE', #854, .T. ) ;
#18873 = LINE ( 'NONE', #18967, #557 ) ;
#18874 = CARTESIAN_POINT ( 'NONE',  ( 47.74827507625478518, 52.59948385550239180, 7.007379884777227730 ) ) ;
#18875 = CARTESIAN_POINT ( 'NONE',  ( -159.0000000000000000, -14.99999999999999645, 17.00000000000000000 ) ) ;
#18876 = CARTESIAN_POINT ( 'NONE',  ( 56.79116909180259398, 63.20051614449766220, 4.963592699178938972 ) ) ;
#18877 = FILL_AREA_STYLE ('',( #8459 ) ) ;
#18878 = EDGE_CURVE ( 'NONE', #6796, #11235, #10598, .T. ) ;
#18879 = CARTESIAN_POINT ( 'NONE',  ( 56.30877334542961421, 63.00051614449766646, 0.02388180880515774693 ) ) ;
#18880 = DIRECTION ( 'NONE',  ( 1.000000000000000000, 0.000000000000000000, 0.000000000000000000 ) ) ;
#18881 = DIRECTION ( 'NONE',  ( 0.6040472319084893016, -0.7969485188038759604, -1.107688701425240097E-17 ) ) ;
#18882 = ORIENTED_EDGE ( 'NONE', *, *, #11926, .T. ) ;
#18883 = ADVANCED_FACE ( 'NONE', ( #4059 ), #1177, .F. ) ;
#18884 = ORIENTED_EDGE ( 'NONE', *, *, #17787, .F. ) ;
#18885 = PLANE ( 'NONE',  #9349 ) ;
#18886 = ORIENTED_EDGE ( 'NONE', *, *, #10943, .T. ) ;
#18887 = EDGE_CURVE ( 'NONE', #11691, #3485, #3863, .T. ) ;
#18888 = EDGE_CURVE ( 'NONE', #12892, #11553, #632, .T. ) ;
#18889 = LINE ( 'NONE', #5424, #7485 ) ;
#18890 = AXIS2_PLACEMENT_3D ( 'NONE', #7990, #12406, #5349 ) ;
#18891 = ORIENTED_EDGE ( 'NONE', *, *, #5329, .T. ) ;
#18892 = DIRECTION ( 'NONE',  ( 0.000000000000000000, -1.000000000000000000, 9.783878858594328898E-16 ) ) ;
#18893 = CARTESIAN_POINT ( 'NONE',  ( 43.33558569842703179, 59.09948385550240602, -2.141517661632099223 ) ) ;
#18894 = ORIENTED_EDGE ( 'NONE', *, *, #11171, .F. ) ;
#18895 = DIRECTION ( 'NONE',  ( 0.000000000000000000, 0.000000000000000000, 1.000000000000000000 ) ) ;
#18896 = EDGE_LOOP ( 'NONE', ( #6805, #14152 ) ) ;
#18897 = CARTESIAN_POINT ( 'NONE',  ( 57.60143344285433642, 59.89948385550240317, -2.493737253992118319 ) ) ;
#18898 = DIRECTION ( 'NONE',  ( 0.000000000000000000, -0.8660254037844380415, 0.5000000000000011102 ) ) ;
#18899 = CARTESIAN_POINT ( 'NONE',  ( 44.91013252490152752, 50.79948385550240175, 3.727524721679198461 ) ) ;
#18900 = CARTESIAN_POINT ( 'NONE',  ( -4.211140560182196957, -2.431303136016552013, -3.745885042887436178 ) ) ;
#18901 = CARTESIAN_POINT ( 'NONE',  ( 12.54977455159103705, -4.427487078051979275, 9.000000000000000000 ) ) ;
#18902 = CARTESIAN_POINT ( 'NONE',  ( 49.97728705011495265, 47.50051614449765935, 8.000000000000001776 ) ) ;
#18903 = EDGE_CURVE ( 'NONE', #7151, #3598, #16620, .T. ) ;
#18904 = CARTESIAN_POINT ( 'NONE',  ( 51.97223112728254790, 64.39948385550239607, 5.992620115222778487 ) ) ;
#18905 = ADVANCED_FACE ( 'NONE', ( #12779, #17402 ), #15824, .T. ) ;
#18906 = CARTESIAN_POINT ( 'NONE',  ( 6.518095160331717430, -2.933089652807539416, 5.080260301817235202 ) ) ;
#18907 = FACE_OUTER_BOUND ( 'NONE', #3994, .T. ) ;
#18908 = ORIENTED_EDGE ( 'NONE', *, *, #14784, .T. ) ;
#18909 = VERTEX_POINT ( 'NONE', #15899 ) ;
#18910 = VERTEX_POINT ( 'NONE', #5325 ) ;
#18911 = CARTESIAN_POINT ( 'NONE',  ( 0.000000000000000000, 0.000000000000000000, -10.00000000000000000 ) ) ;
#18912 = ORIENTED_EDGE ( 'NONE', *, *, #17114, .T. ) ;
#18913 = CARTESIAN_POINT ( 'NONE',  ( 56.66441430157296821, 58.09948385550240602, 2.141517661632100111 ) ) ;
#18914 = DIRECTION ( 'NONE',  ( -0.000000000000000000, -0.000000000000000000, 1.000000000000000000 ) ) ;
#18915 = ORIENTED_EDGE ( 'NONE', *, *, #3055, .T. ) ;
#18916 = VERTEX_POINT ( 'NONE', #920 ) ;
#18917 = CYLINDRICAL_SURFACE ( 'NONE', #19311, 1.000000000000000888 ) ;
#18918 = ORIENTED_EDGE ( 'NONE', *, *, #11192, .T. ) ;
#18919 = FACE_OUTER_BOUND ( 'NONE', #11527, .T. ) ;
#18920 = ORIENTED_EDGE ( 'NONE', *, *, #1026, .T. ) ;
#18921 = CARTESIAN_POINT ( 'NONE',  ( 47.74827507625478518, 54.59948385550239180, 7.007379884777227730 ) ) ;
#18922 = CARTESIAN_POINT ( 'NONE',  ( 8.500000000000000000, -2.886751345948133984, -5.000000000000000000 ) ) ;
#18923 = CARTESIAN_POINT ( 'NONE',  ( 52.25172492374527877, 47.40051614449766504, 7.007379884777203749 ) ) ;
#18924 = LINE ( 'NONE', #15775, #11098 ) ;
#18925 = DIRECTION ( 'NONE',  ( 0.5000000000000108802, -0.8660254037844323793, 0.000000000000000000 ) ) ;
#18926 = EDGE_CURVE ( 'NONE', #10552, #12060, #6891, .T. ) ;
#18927 = CARTESIAN_POINT ( 'NONE',  ( 0.1381419387119174058, -1.355287006778759018, 3.500000000000000888 ) ) ;
#18928 = CIRCLE ( 'NONE', #16415, 20.00000000000000000 ) ;
#18929 = EDGE_CURVE ( 'NONE', #7086, #928, #335, .T. ) ;
#18930 = ORIENTED_EDGE ( 'NONE', *, *, #13338, .T. ) ;
#18931 = VERTEX_POINT ( 'NONE', #4343 ) ;
#18932 = CARTESIAN_POINT ( 'NONE',  ( 4.175813232069147674, 2.061359961916367833, 3.570380186727398097 ) ) ;
#18933 =( NAMED_UNIT ( * ) PLANE_ANGLE_UNIT ( ) SI_UNIT ( $, .RADIAN. ) );
#18934 = CIRCLE ( 'NONE', #7010, 3.799999999999993605 ) ;
#18935 = LINE ( 'NONE', #14295, #6481 ) ;
#18936 = CARTESIAN_POINT ( 'NONE',  ( 2.649999999999988365, 15.00000000000001599, 15.00000000000000000 ) ) ;
#18937 = ORIENTED_EDGE ( 'NONE', *, *, #10706, .T. ) ;
#18938 = CARTESIAN_POINT ( 'NONE',  ( 6.385552186430389021, 5.773502691896261751, 0.000000000000000000 ) ) ;
#18939 = ORIENTED_EDGE ( 'NONE', *, *, #1976, .T. ) ;
#18940 = ORIENTED_EDGE ( 'NONE', *, *, #2015, .F. ) ;
#18941 = ADVANCED_FACE ( 'NONE', ( #7573 ), #8778, .T. ) ;
#18942 = VECTOR ( 'NONE', #12957, 1000.000000000000114 ) ;
#18943 = FACE_OUTER_BOUND ( 'NONE', #18717, .T. ) ;
#18944 = PLANE ( 'NONE',  #13617 ) ;
#18945 = CIRCLE ( 'NONE', #2027, 2.649999999999988365 ) ;
#18946 = CARTESIAN_POINT ( 'NONE',  ( 55.71335778527780036, 50.90051614449765793, -1.832500667257213056 ) ) ;
#18947 = CARTESIAN_POINT ( 'NONE',  ( 5.599999999999999645, -4.041451884327386779, 0.000000000000000000 ) ) ;
#18948 = EDGE_CURVE ( 'NONE', #7769, #13093, #11600, .T. ) ;
#18949 = CARTESIAN_POINT ( 'NONE',  ( 4.093692494532771953, 2.021783646005768542, 3.501831996793843160 ) ) ;
#18950 = CARTESIAN_POINT ( 'NONE',  ( 55.08986747509847248, 51.79948385550240175, -3.727524721679197572 ) ) ;
#18951 = CARTESIAN_POINT ( 'NONE',  ( 0.2174200650117547873, 3.876582599186211731, 0.2855619784720684895 ) ) ;
#18952 = CARTESIAN_POINT ( 'NONE',  ( 52.57664461997811856, 63.59948385550239891, -8.007379884777229506 ) ) ;
#18953 = CARTESIAN_POINT ( 'NONE',  ( 56.79116909180259398, 49.20051614449766220, 4.963592699178938972 ) ) ;
#18954 = CARTESIAN_POINT ( 'NONE',  ( 5.130877905917419213, -39.33065161639846252, 9.000000000000000000 ) ) ;
#18955 = CARTESIAN_POINT ( 'NONE',  ( 0.000000000000000000, 0.5192545390863916310, -1.000000000000000000 ) ) ;
#18956 = CARTESIAN_POINT ( 'NONE',  ( 3.851859888774471706E-31, 15.00000000000001599, -20.00000000000000000 ) ) ;
#18957 = EDGE_LOOP ( 'NONE', ( #15111, #1946, #9718, #17500 ) ) ;
#18958 = CIRCLE ( 'NONE', #7038, 1.000000000000000222 ) ;
#18959 = DIRECTION ( 'NONE',  ( 0.000000000000000000, 0.000000000000000000, 1.000000000000000000 ) ) ;
#18960 = DIRECTION ( 'NONE',  ( -9.858538378746663627E-23, 5.031452844637890958E-23, -1.000000000000000000 ) ) ;
#18961 = CARTESIAN_POINT ( 'NONE',  ( 44.03140696652198471, 51.80051614449766362, 4.306917132069485454 ) ) ;
#18962 = AXIS2_PLACEMENT_3D ( 'NONE', #12009, #2820, #4674 ) ;
#18963 = DIRECTION ( 'NONE',  ( -1.000000000000000000, 0.000000000000000000, 0.000000000000000000 ) ) ;
#18964 = CARTESIAN_POINT ( 'NONE',  ( 55.00886502606627459, 44.74918607449495767, -5.000000000000008882 ) ) ;
#18965 = ORIENTED_EDGE ( 'NONE', *, *, #17501, .T. ) ;
#18966 = LINE ( 'NONE', #3952, #7953 ) ;
#18967 = CARTESIAN_POINT ( 'NONE',  ( 1.171083334267915221, -24.65495046420793201, 9.000000000000000000 ) ) ;
#18968 = CARTESIAN_POINT ( 'NONE',  ( 45.86712807150323812, 51.29948385550240175, -5.649768623646098220 ) ) ;
#18969 = CIRCLE ( 'NONE', #15501, 0.7499999999999997780 ) ;
#18970 = DIRECTION ( 'NONE',  ( 1.000000000000000000, 0.000000000000000000, 0.000000000000000000 ) ) ;
#18971 = CARTESIAN_POINT ( 'NONE',  ( 50.02271294988505446, 64.50051614449766646, -8.000000000000001776 ) ) ;
#18972 = CARTESIAN_POINT ( 'NONE',  ( -3.799999999999999378, 4.653657836759941744E-16, -0.8000000000000000444 ) ) ;
#18973 = CARTESIAN_POINT ( 'NONE',  ( 43.34962307344078880, 46.10051614449766078, -2.184720259617096705 ) ) ;
#18974 = FACE_OUTER_BOUND ( 'NONE', #8044, .T. ) ;
#18975 = FACE_OUTER_BOUND ( 'NONE', #1922, .T. ) ;
#18976 = AXIS2_PLACEMENT_3D ( 'NONE', #8319, #15787, #12546 ) ;
#18977 = ORIENTED_EDGE ( 'NONE', *, *, #8435, .T. ) ;
#18978 = ORIENTED_EDGE ( 'NONE', *, *, #18257, .F. ) ;
#18979 = DIRECTION ( 'NONE',  ( 0.000000000000000000, 0.000000000000000000, 1.000000000000000000 ) ) ;
#18980 = ORIENTED_EDGE ( 'NONE', *, *, #4020, .T. ) ;
#18981 = CARTESIAN_POINT ( 'NONE',  ( -4.000000000000000000, 0.7924765000094600165, -0.05906175389889745803 ) ) ;
#18982 = ORIENTED_EDGE ( 'NONE', *, *, #4749, .T. ) ;
#18983 = CARTESIAN_POINT ( 'NONE',  ( 62.49999999999998579, 32.50000000000001421, 15.00000000000000000 ) ) ;
#18984 = EDGE_CURVE ( 'NONE', #14141, #5072, #8154, .T. ) ;
#18985 = CARTESIAN_POINT ( 'NONE',  ( 55.94051828345050836, 59.79948385550240175, -4.345558710429103577 ) ) ;
#18986 = ORIENTED_EDGE ( 'NONE', *, *, #7733, .T. ) ;
#18987 = CARTESIAN_POINT ( 'NONE',  ( 0.8816464618332836567, -24.71833652004169934, 9.000000000000000000 ) ) ;
#18988 = EDGE_LOOP ( 'NONE', ( #8503, #15375, #16781, #9494 ) ) ;
#18989 = CARTESIAN_POINT ( 'NONE',  ( 42.38452918213188525, 61.09948385550241312, -2.450534656007040013 ) ) ;
#18990 = CARTESIAN_POINT ( 'NONE',  ( 0.2174200650117528444, 2.185595227304856891, -3.214438021527932676 ) ) ;
#18991 = AXIS2_PLACEMENT_3D ( 'NONE', #18040, #1461, #15178 ) ;
#18992 = EDGE_CURVE ( 'NONE', #4430, #1140, #5026, .T. ) ;
#18993 = CARTESIAN_POINT ( 'NONE',  ( 53.54508667620428497, 48.29948385550240175, 4.840751629271157874 ) ) ;
#18994 = CARTESIAN_POINT ( 'NONE',  ( -144.9999999999999716, -14.99999999999999467, 4.000000000000000000 ) ) ;
#18995 = PLANE ( 'NONE',  #6798 ) ;
#18996 = CARTESIAN_POINT ( 'NONE',  ( 42.38452918213190657, 49.90051614449766504, 2.450534656007115508 ) ) ;
#18997 = EDGE_CURVE ( 'NONE', #2159, #16413, #8471, .T. ) ;
#18998 = CARTESIAN_POINT ( 'NONE',  ( 44.28664221472221385, 49.90051614449766504, 1.832500667257213722 ) ) ;
#18999 = EDGE_CURVE ( 'NONE', #4627, #3135, #14723, .T. ) ;
#19000 = AXIS2_PLACEMENT_3D ( 'NONE', #15382, #15189, #1962 ) ;
#19001 = DIRECTION ( 'NONE',  ( 0.000000000000000000, 0.000000000000000000, 1.000000000000000000 ) ) ;
#19002 = CARTESIAN_POINT ( 'NONE',  ( 2.449293598294706513E-15, -20.00000000000000000, 9.000000000000000000 ) ) ;
#19003 = ORIENTED_EDGE ( 'NONE', *, *, #12790, .T. ) ;
#19004 = EDGE_CURVE ( 'NONE', #11693, #11530, #12850, .T. ) ;
#19005 = EDGE_LOOP ( 'NONE', ( #5079, #4816, #11784, #1027 ) ) ;
#19006 = CARTESIAN_POINT ( 'NONE',  ( -19.76107906696391225, -16.91783288752853665, 0.000000000000000000 ) ) ;
#19007 =( NAMED_UNIT ( * ) PLANE_ANGLE_UNIT ( ) SI_UNIT ( $, .RADIAN. ) );
#19008 = ORIENTED_EDGE ( 'NONE', *, *, #7602, .T. ) ;
#19009 = CARTESIAN_POINT ( 'NONE',  ( 56.65037692655918988, 57.89948385550240317, -2.184720259617163762 ) ) ;
#19010 = SURFACE_STYLE_FILL_AREA ( #1054 ) ;
#19011 = ORIENTED_EDGE ( 'NONE', *, *, #5020, .F. ) ;
#19012 = VERTEX_POINT ( 'NONE', #8751 ) ;
#19013 = FACE_OUTER_BOUND ( 'NONE', #7220, .T. ) ;
#19014 = EDGE_CURVE ( 'NONE', #11065, #13816, #13488, .T. ) ;
#19015 = EDGE_CURVE ( 'NONE', #19163, #4462, #14728, .T. ) ;
#19016 = ORIENTED_EDGE ( 'NONE', *, *, #4237, .F. ) ;
#19017 = CARTESIAN_POINT ( 'NONE',  ( 0.1983443223721582938, 5.300482436767278038, 0.8192951148925896598 ) ) ;
#19018 = ORIENTED_EDGE ( 'NONE', *, *, #5411, .F. ) ;
#19019 = CARTESIAN_POINT ( 'NONE',  ( 54.13287192849676188, 50.29948385550240175, 5.649768623646098220 ) ) ;
#19020 = DIRECTION ( 'NONE',  ( 0.000000000000000000, 0.000000000000000000, -1.000000000000000000 ) ) ;
#19021 = AXIS2_PLACEMENT_3D ( 'NONE', #5029, #11001, #9526 ) ;
#19022 = CARTESIAN_POINT ( 'NONE',  ( 50.02271294988505446, 46.50051614449765935, -7.000000000000000888 ) ) ;
#19023 = DIRECTION ( 'NONE',  ( 1.000000000000000000, 0.000000000000000000, 0.000000000000000000 ) ) ;
#19024 = EDGE_CURVE ( 'NONE', #444, #6110, #30, .T. ) ;
#19025 = CARTESIAN_POINT ( 'NONE',  ( 62.49999999999998579, 5.000000000000018652, 5.000000000000000000 ) ) ;
#19026 = DIRECTION ( 'NONE',  ( 0.000000000000000000, 0.000000000000000000, 1.000000000000000000 ) ) ;
#19027 = AXIS2_PLACEMENT_3D ( 'NONE', #7565, #18071, #16307 ) ;
#19028 = PRODUCT_DEFINITION_SHAPE ( 'NONE', 'NONE',  #19435 ) ;
#19029 = ORIENTED_EDGE ( 'NONE', *, *, #7417, .T. ) ;
#19030 = EDGE_LOOP ( 'NONE', ( #5165, #16462, #17347, #19059 ) ) ;
#19031 = CARTESIAN_POINT ( 'NONE',  ( -62.49999999999997158, 32.50000000000001421, 10.00000000000000000 ) ) ;
#19032 = CIRCLE ( 'NONE', #9907, 0.7500000000000000000 ) ;
#19033 = CARTESIAN_POINT ( 'NONE',  ( 0.000000000000000000, 4.330127018922190985, 2.500000000000005329 ) ) ;
#19034 = CARTESIAN_POINT ( 'NONE',  ( 19.76107906696387673, -16.91783288752826664, 0.000000000000000000 ) ) ;
#19035 = VERTEX_POINT ( 'NONE', #1211 ) ;
#19036 = AXIS2_PLACEMENT_3D ( 'NONE', #13015, #11728, #2741 ) ;
#19037 = DIRECTION ( 'NONE',  ( 0.000000000000000000, 0.000000000000000000, -1.000000000000000000 ) ) ;
#19038 = VERTEX_POINT ( 'NONE', #17986 ) ;
#19039 = ORIENTED_EDGE ( 'NONE', *, *, #651, .T. ) ;
#19040 = CARTESIAN_POINT ( 'NONE',  ( 8.134732861515777458, -1.729090847147875198, -9.000000000000000000 ) ) ;
#19041 = CARTESIAN_POINT ( 'NONE',  ( 0.2182387239012630320, 1.693823289460900883, -3.499999999999999112 ) ) ;
#19042 = CIRCLE ( 'NONE', #10553, 2.649999999999985700 ) ;
#19043 = CARTESIAN_POINT ( 'NONE',  ( 49.97728705011494554, 51.50051614449765935, 6.000000000000000888 ) ) ;
#19044 = DIRECTION ( 'NONE',  ( 0.000000000000000000, 0.8660254037844375974, -0.5000000000000018874 ) ) ;
#19045 = AXIS2_PLACEMENT_3D ( 'NONE', #5407, #809, #12955 ) ;
#19046 = DIRECTION ( 'NONE',  ( 0.000000000000000000, 0.000000000000000000, -1.000000000000000000 ) ) ;
#19047 = CARTESIAN_POINT ( 'NONE',  ( 49.97728705011488870, 49.49948385550241170, -6.000000000000000888 ) ) ;
#19048 = CARTESIAN_POINT ( 'NONE',  ( 0.000000000000000000, 3.031088913245533867, 1.750000000000002887 ) ) ;
#19049 = COLOUR_RGB ( '',1.000000000000000000, 0.9490196078431372140, 0.9098039215686274384 ) ;
#19050 = CARTESIAN_POINT ( 'NONE',  ( 55.94051828345050836, 45.79948385550240886, -4.345558710429104465 ) ) ;
#19051 = CARTESIAN_POINT ( 'NONE',  ( 52.57664461997821093, 47.40051614449765793, 8.007379884777206414 ) ) ;
#19052 = DIRECTION ( 'NONE',  ( 1.000000000000000000, 0.000000000000000000, 0.000000000000000000 ) ) ;
#19053 = CARTESIAN_POINT ( 'NONE',  ( -1.000000000000000000, -6.008326913195983998, 0.000000000000000000 ) ) ;
#19054 =( NAMED_UNIT ( * ) PLANE_ANGLE_UNIT ( ) SI_UNIT ( $, .RADIAN. ) );
#19055 = ADVANCED_FACE ( 'NONE', ( #13556, #11687 ), #14828, .T. ) ;
#19056 = B_SPLINE_CURVE_WITH_KNOTS ( 'NONE', 3,
 ( #14279, #17444, #15570, #8214, #17251, #5271, #13985, #17057 ),
 .UNSPECIFIED., .F., .F.,
 ( 4, 2, 2, 4 ),
 ( 0.005725059856848645212, 0.006314084072593634418, 0.006903108288338624492, 0.008081156719828603771 ),
 .UNSPECIFIED. ) ;
#19057 = DIRECTION ( 'NONE',  ( 1.000000000000000000, 0.000000000000000000, 0.000000000000000000 ) ) ;
#19058 = CIRCLE ( 'NONE', #10262, 1.000000000000000444 ) ;
#19059 = ORIENTED_EDGE ( 'NONE', *, *, #5807, .F. ) ;
#19060 = CARTESIAN_POINT ( 'NONE',  ( 2.449293598294706513E-15, -20.00000000000000000, 9.000000000000000000 ) ) ;
#19061 = EDGE_CURVE ( 'NONE', #4701, #12235, #15999, .T. ) ;
#19062 = AXIS2_PLACEMENT_3D ( 'NONE', #11757, #8833, #8730 ) ;
#19063 = DIRECTION ( 'NONE',  ( -0.9768494444668812671, -0.2139279384389642935, 0.000000000000000000 ) ) ;
#19064 = CARTESIAN_POINT ( 'NONE',  ( 57.36023556966787851, 51.00051614449765225, 0.02388180880515038476 ) ) ;
#19065 = DIRECTION ( 'NONE',  ( 1.000000000000000000, 0.000000000000000000, -0.000000000000000000 ) ) ;
#19066 = CYLINDRICAL_SURFACE ( 'NONE', #16197, 5.575000000000000178 ) ;
#19067 = EDGE_LOOP ( 'NONE', ( #3607, #2348, #12894, #484 ) ) ;
#19068 = DIRECTION ( 'NONE',  ( -0.000000000000000000, -0.000000000000000000, 1.000000000000000000 ) ) ;
#19069 = DIRECTION ( 'NONE',  ( 0.000000000000000000, -1.000000000000000000, 0.000000000000000000 ) ) ;
#19070 = CARTESIAN_POINT ( 'NONE',  ( 56.66441430157296821, 50.09948385550240602, 2.141517661632100111 ) ) ;
#19071 = CARTESIAN_POINT ( 'NONE',  ( 0.000000000000000000, 0.000000000000000000, 5.000000000000000000 ) ) ;
#19072 = CARTESIAN_POINT ( 'NONE',  ( 43.20883090819745576, 46.79948385550240886, 4.963592699179006473 ) ) ;
#19073 = DIRECTION ( 'NONE',  ( -0.3090169943749382919, -0.9510565162951566398, 0.000000000000000000 ) ) ;
#19074 = CARTESIAN_POINT ( 'NONE',  ( 52.29715082351538769, 48.60051614449766788, -6.992620115222796251 ) ) ;
#19075 = CIRCLE ( 'NONE', #10890, 20.00000000000000000 ) ;
#19076 =( REPRESENTATION_RELATIONSHIP ('NONE','NONE', #16703, #4039 ) REPRESENTATION_RELATIONSHIP_WITH_TRANSFORMATION ( #11255 )SHAPE_REPRESENTATION_RELATIONSHIP( ) );
#19077 = CARTESIAN_POINT ( 'NONE',  ( 6.207682235857189035, 2.016324304256315258, 4.999999999999999112 ) ) ;
#19078 = ORIENTED_EDGE ( 'NONE', *, *, #14355, .F. ) ;
#19079 = PRESENTATION_LAYER_ASSIGNMENT (  '', '', ( #4971 ) ) ;
#19080 = ORIENTED_EDGE ( 'NONE', *, *, #10953, .T. ) ;
#19081 = LINE ( 'NONE', #9212, #10917 ) ;
#19082 = EDGE_LOOP ( 'NONE', ( #1821, #2410 ) ) ;
#19083 = CARTESIAN_POINT ( 'NONE',  ( -72.99999999999997158, -3.000000000000000000, -20.00000000000000000 ) ) ;
#19084 = ORIENTED_EDGE ( 'NONE', *, *, #8199, .F. ) ;
#19085 = DIRECTION ( 'NONE',  ( 1.000000000000000000, 0.000000000000000000, 0.000000000000000000 ) ) ;
#19086 = COLOUR_RGB ( '',0.8941176470588234615, 0.8941176470588234615, 0.8941176470588234615 ) ;
#19087 = CIRCLE ( 'NONE', #8405, 12.49999999999999645 ) ;
#19088 = VERTEX_POINT ( 'NONE', #7286 ) ;
#19089 = CARTESIAN_POINT ( 'NONE',  ( 0.1973348417602843741, -1.936114729415326696, -5.000000000000000000 ) ) ;
#19090 = EDGE_LOOP ( 'NONE', ( #5840, #8498, #4502, #18221 ) ) ;
#19091 = CARTESIAN_POINT ( 'NONE',  ( 42.38452918213188525, 57.09948385550240602, -2.450534656007040013 ) ) ;
#19092 = FACE_OUTER_BOUND ( 'NONE', #15444, .T. ) ;
#19093 = CARTESIAN_POINT ( 'NONE',  ( 53.54508667620428497, 52.29948385550240886, 4.840751629271157874 ) ) ;
#19094 = CARTESIAN_POINT ( 'NONE',  ( 5.686050877451574337, -5.768780236673276995, 0.000000000000000000 ) ) ;
#19095 = DIRECTION ( 'NONE',  ( -1.000000000000000000, 0.000000000000000000, 0.000000000000000000 ) ) ;
#19096 = AXIS2_PLACEMENT_3D ( 'NONE', #8541, #5401, #15802 ) ;
#19097 = CARTESIAN_POINT ( 'NONE',  ( 45.27934281921082516, 47.70051614449766220, 6.458785618021089192 ) ) ;
#19098 = CARTESIAN_POINT ( 'NONE',  ( 55.11794222512599362, 46.80051614449766362, -3.688883143319583446 ) ) ;
#19099 = DIRECTION ( 'NONE',  ( -1.000000000000000000, -4.082155997157843695E-16, 0.000000000000000000 ) ) ;
#19100 = CARTESIAN_POINT ( 'NONE',  ( 13.99999999999999822, 2.210487472460973684E-16, -1.610000000000000098 ) ) ;
#19101 = VECTOR ( 'NONE', #6390, 1000.000000000000000 ) ;
#19102 = EDGE_CURVE ( 'NONE', #18783, #8359, #17785, .T. ) ;
#19103 = ORIENTED_EDGE ( 'NONE', *, *, #4125, .F. ) ;
#19104 = VECTOR ( 'NONE', #18011, 1000.000000000000000 ) ;
#19105 = ORIENTED_EDGE ( 'NONE', *, *, #14050, .T. ) ;
#19106 = DIRECTION ( 'NONE',  ( 0.000000000000000000, -1.000000000000000000, -0.000000000000000000 ) ) ;
#19107 =( NAMED_UNIT ( * ) PLANE_ANGLE_UNIT ( ) SI_UNIT ( $, .RADIAN. ) );
#19108 = ORIENTED_EDGE ( 'NONE', *, *, #102, .F. ) ;
#19109 = CARTESIAN_POINT ( 'NONE',  ( 55.94051828345050836, 55.79948385550238044, -4.345558710429104465 ) ) ;
#19110 = AXIS2_PLACEMENT_3D ( 'NONE', #2391, #6874, #12865 ) ;
#19111 = VERTEX_POINT ( 'NONE', #10504 ) ;
#19112 = ORIENTED_EDGE ( 'NONE', *, *, #7696, .F. ) ;
#19113 = DIRECTION ( 'NONE',  ( -0.9396926207859138680, 0.000000000000000000, -0.3420201433256536139 ) ) ;
#19114 = CYLINDRICAL_SURFACE ( 'NONE', #22, 24.99999999999999289 ) ;
#19115 = ORIENTED_EDGE ( 'NONE', *, *, #18301, .F. ) ;
#19116 = CARTESIAN_POINT ( 'NONE',  ( 2.649999999999989697, 15.00000000000001599, -9.000000000000001776 ) ) ;
#19117 = ORIENTED_EDGE ( 'NONE', *, *, #2519, .F. ) ;
#19118 = CARTESIAN_POINT ( 'NONE',  ( -154.9999999999999716, -14.99999999999999645, 9.000000000000000000 ) ) ;
#19119 = CARTESIAN_POINT ( 'NONE',  ( 44.03140696652192787, 51.19948385550238612, -4.306917132069425058 ) ) ;
#19120 = CARTESIAN_POINT ( 'NONE',  ( 14.14213562373094923, -14.99999999999999112, -23.00000000000000000 ) ) ;
#19121 = EDGE_CURVE ( 'NONE', #9774, #12905, #12544, .T. ) ;
#19122 = CARTESIAN_POINT ( 'NONE',  ( 54.09612160359792199, 47.30051614449765651, 5.676469297603124353 ) ) ;
#19123 = LINE ( 'NONE', #1353, #9853 ) ;
#19124 = VECTOR ( 'NONE', #4715, 1000.000000000000000 ) ;
#19125 = CARTESIAN_POINT ( 'NONE',  ( 0.000000000000000000, 0.000000000000000000, 0.000000000000000000 ) ) ;
#19126 = EDGE_CURVE ( 'NONE', #3492, #8944, #5814, .T. ) ;
#19127 = EDGE_CURVE ( 'NONE', #17949, #2897, #16508, .T. ) ;
#19128 = ORIENTED_EDGE ( 'NONE', *, *, #15518, .T. ) ;
#19129 = EDGE_LOOP ( 'NONE', ( #7312, #19414 ) ) ;
#19130 = CARTESIAN_POINT ( 'NONE',  ( -154.9999999999999716, -14.99999999999999645, 15.00000000000000000 ) ) ;
#19131 = PRESENTATION_STYLE_ASSIGNMENT (( #4301 ) ) ;
#19132 = AXIS2_PLACEMENT_3D ( 'NONE', #8027, #5286, #14003 ) ;
#19133 = CARTESIAN_POINT ( 'NONE',  ( -74.99999999999997158, -23.00000000000000355, 15.00000000000000000 ) ) ;
#19134 = SURFACE_STYLE_FILL_AREA ( #18842 ) ;
#19135 = VECTOR ( 'NONE', #13236, 1000.000000000000000 ) ;
#19136 = CIRCLE ( 'NONE', #16616, 5.575000000000000178 ) ;
#19137 = ORIENTED_EDGE ( 'NONE', *, *, #5209, .T. ) ;
#19138 = DIRECTION ( 'NONE',  ( 0.000000000000000000, 0.000000000000000000, 1.000000000000000000 ) ) ;
#19139 = ADVANCED_FACE ( 'NONE', ( #17602 ), #8852, .F. ) ;
#19140 = AXIS2_PLACEMENT_3D ( 'NONE', #10143, #17331, #3890 ) ;
#19141 = EDGE_LOOP ( 'NONE', ( #13525, #8478, #1058, #2412 ) ) ;
#19142 = ORIENTED_EDGE ( 'NONE', *, *, #18187, .F. ) ;
#19143 = DIRECTION ( 'NONE',  ( -0.000000000000000000, -0.000000000000000000, 1.000000000000000000 ) ) ;
#19144 = PRODUCT_DEFINITION_CONTEXT ( 'detailed design', #12034, 'design' ) ;
#19146 = CIRCLE ( 'NONE', #16949, 0.9999999999999982236 ) ;
#19145 = CARTESIAN_POINT ( 'NONE',  ( 48.02776887271750184, 51.60051614449766788, 5.992620115222795363 ) ) ;
#19147 = CARTESIAN_POINT ( 'NONE',  ( 22.00000000000000000, -20.00000000000000000, -12.00000000000000000 ) ) ;
#19148 = DIRECTION ( 'NONE',  ( -0.000000000000000000, 0.000000000000000000, -1.000000000000000000 ) ) ;
#19149 = CARTESIAN_POINT ( 'NONE',  ( 50.02271294988511841, 50.49948385550239749, 6.000000000000000888 ) ) ;
#19150 = CIRCLE ( 'NONE', #12845, 4.999999999999999112 ) ;
#19151 = CARTESIAN_POINT ( 'NONE',  ( 3.806834918298644954, -3.031088913245541416, -1.749999999999998890 ) ) ;
#19152 = AXIS2_PLACEMENT_3D ( 'NONE', #13177, #1324, #6116 ) ;
#19153 = CARTESIAN_POINT ( 'NONE',  ( 43.34962307344081012, 50.89948385550241028, 2.184720259617164650 ) ) ;
#19154 = ADVANCED_FACE ( 'NONE', ( #15503 ), #4920, .F. ) ;
#19155 = CARTESIAN_POINT ( 'NONE',  ( 42.39856655714564226, 48.10051614449766078, -2.493737253992044156 ) ) ;
#19156 = CARTESIAN_POINT ( 'NONE',  ( -129.9999999999999716, -14.99999999999999645, 3.999999999999999112 ) ) ;
#19157 = EDGE_CURVE ( 'NONE', #6680, #228, #2852, .T. ) ;
#19158 = AXIS2_PLACEMENT_3D ( 'NONE', #14927, #4157, #1503 ) ;
#19159 = EDGE_LOOP ( 'NONE', ( #13078, #4458, #10486, #8855 ) ) ;
#19160 = DIRECTION ( 'NONE',  ( 0.000000000000000000, 0.000000000000000000, 1.000000000000000000 ) ) ;
#19161 = PRESENTATION_STYLE_ASSIGNMENT (( #4432 ) ) ;
#19162 = DIRECTION ( 'NONE',  ( 0.9999419836444146670, 0.01077169184824074144, -2.272467923560868902E-17 ) ) ;
#19163 = VERTEX_POINT ( 'NONE', #1699 ) ;
#19164 = CIRCLE ( 'NONE', #10003, 0.9999999999999995559 ) ;
#19165 = DIRECTION ( 'NONE',  ( 0.000000000000000000, 0.000000000000000000, 1.000000000000000000 ) ) ;
#19166 = DIRECTION ( 'NONE',  ( -1.000000000000000000, 0.000000000000000000, 0.000000000000000000 ) ) ;
#19167 = AXIS2_PLACEMENT_3D ( 'NONE', #17641, #17730, #17439 ) ;
#19168 = CIRCLE ( 'NONE', #18531, 4.000000000000000000 ) ;
#19169 = CARTESIAN_POINT ( 'NONE',  ( 6.244004651191001010, -4.663678638742299931, -2.132808149174403312 ) ) ;
#19170 = DIRECTION ( 'NONE',  ( 1.000000000000000000, 0.000000000000000000, 0.000000000000000000 ) ) ;
#19171 = ORIENTED_EDGE ( 'NONE', *, *, #14917, .T. ) ;
#19172 = CARTESIAN_POINT ( 'NONE',  ( -65.14999999999996305, 32.50000000000001421, 9.999999999999998224 ) ) ;
#19173 = EDGE_CURVE ( 'NONE', #4901, #17113, #10703, .T. ) ;
#19174 = CARTESIAN_POINT ( 'NONE',  ( 0.6810597143197052450, 4.461075778259290914, -3.598441714920602053 ) ) ;
#19175 = CARTESIAN_POINT ( 'NONE',  ( 49.97728705011488159, 51.49948385550240459, -7.000000000000000888 ) ) ;
#19176 = DIRECTION ( 'NONE',  ( 0.000000000000000000, 0.000000000000000000, 1.000000000000000000 ) ) ;
#19177 = CARTESIAN_POINT ( 'NONE',  ( 47.37792948025162332, 49.39948385550241028, -7.992620115222770494 ) ) ;
#19178 = DIRECTION ( 'NONE',  ( 0.000000000000000000, 1.000000000000000000, -1.345283343056720273E-15 ) ) ;
#19179 = EDGE_CURVE ( 'NONE', #12796, #11041, #3361, .T. ) ;
#19180 = CARTESIAN_POINT ( 'NONE',  ( 54.09612160359792199, 49.30051614449765651, 5.676469297603124353 ) ) ;
#19181 = AXIS2_PLACEMENT_3D ( 'NONE', #12307, #4867, #5630 ) ;
#19182 = DIRECTION ( 'NONE',  ( 0.000000000000000000, 0.000000000000000000, 1.000000000000000000 ) ) ;
#19183 = VECTOR ( 'NONE', #11368, 1000.000000000000000 ) ;
#19184 = ORIENTED_EDGE ( 'NONE', *, *, #4836, .F. ) ;
#19185=STYLED_ITEM('',(#19475),#2357);
#19186 = ORIENTED_EDGE ( 'NONE', *, *, #12800, .T. ) ;
#19187 = DIRECTION ( 'NONE',  ( -0.000000000000000000, 0.000000000000000000, 1.000000000000000000 ) ) ;
#19188 = ORIENTED_EDGE ( 'NONE', *, *, #3423, .T. ) ;
#19189 = DIRECTION ( 'NONE',  ( -0.000000000000000000, -0.000000000000000000, -1.000000000000000000 ) ) ;
#19190 = VERTEX_POINT ( 'NONE', #16795 ) ;
#19191 = DIRECTION ( 'NONE',  ( -0.000000000000000000, -0.000000000000000000, -1.000000000000000000 ) ) ;
#19192 = ORIENTED_EDGE ( 'NONE', *, *, #18948, .T. ) ;
#19193 = CARTESIAN_POINT ( 'NONE',  ( 50.02271294988505446, 64.50051614449765225, -7.000000000000000888 ) ) ;
#19194 = ORIENTED_EDGE ( 'NONE', *, *, #7051, .T. ) ;
#19195 = CARTESIAN_POINT ( 'NONE',  ( 43.18075615816989199, 57.19948385550241454, -4.924951120819313743 ) ) ;
#19196 = LINE ( 'NONE', #14459, #2656 ) ;
#19197 = ADVANCED_FACE ( 'NONE', ( #9323 ), #3265, .F. ) ;
#19198 = PRODUCT_DEFINITION_SHAPE ( 'NONE', 'NONE',  #10089 ) ;
#19199 = CARTESIAN_POINT ( 'NONE',  ( 43.69122665457040000, 52.99948385550241170, 0.02388180880521036456 ) ) ;
#19200 = DIRECTION ( 'NONE',  ( -1.000000000000000000, 0.000000000000000000, 0.000000000000000000 ) ) ;
#19201 = CARTESIAN_POINT ( 'NONE',  ( 5.599999999999999645, -2.020725942163694722, -3.499999999999999556 ) ) ;
#19202 = CARTESIAN_POINT ( 'NONE',  ( 54.68390685589039890, 45.30051614449766362, 6.485486291978072693 ) ) ;
#19203 = CARTESIAN_POINT ( 'NONE',  ( 51.92680522751238925, 51.40051614449767214, 6.007379884777208190 ) ) ;
#19204 = DIRECTION ( 'NONE',  ( -1.000000000000000000, 0.000000000000000000, 0.000000000000000000 ) ) ;
#19205 = FACE_OUTER_BOUND ( 'NONE', #8361, .T. ) ;
#19206 = VERTEX_POINT ( 'NONE', #3460 ) ;
#19207 = VECTOR ( 'NONE', #4758, 1000.000000000000000 ) ;
#19208 = ORIENTED_EDGE ( 'NONE', *, *, #17697, .F. ) ;
#19209 = CARTESIAN_POINT ( 'NONE',  ( 2.595115354961440524, -7.673029147243177306, -1.000000000000000000 ) ) ;
#19210 = ORIENTED_EDGE ( 'NONE', *, *, #6389, .T. ) ;
#19211 = CARTESIAN_POINT ( 'NONE',  ( 56.66441430157296821, 62.09948385550239891, 2.141517661632100111 ) ) ;
#19212 = CARTESIAN_POINT ( 'NONE',  ( -20.00000000000000000, -19.99999999999999289, -23.00000000000000000 ) ) ;
#19213 = VERTEX_POINT ( 'NONE', #4743 ) ;
#19214 = ORIENTED_EDGE ( 'NONE', *, *, #11972, .F. ) ;
#19215 = DIRECTION ( 'NONE',  ( -0.000000000000000000, -0.000000000000000000, -1.000000000000000000 ) ) ;
#19216 = CARTESIAN_POINT ( 'NONE',  ( 52.25172492374522903, 47.59948385550240602, -7.007379884777227730 ) ) ;
#19217 = EDGE_LOOP ( 'NONE', ( #13194, #7609, #6021, #1611 ) ) ;
#19218 = CYLINDRICAL_SURFACE ( 'NONE', #18223, 3.799999999999999378 ) ;
#19219 = ORIENTED_EDGE ( 'NONE', *, *, #17077, .T. ) ;
#19220 = CARTESIAN_POINT ( 'NONE',  ( 20.00000000000000000, -14.99999999999999289, -23.00000000000000000 ) ) ;
#19221 = CARTESIAN_POINT ( 'NONE',  ( 45.90387839640214196, 54.69948385550240744, 5.676469297603166098 ) ) ;
#19222 = LINE ( 'NONE', #1259, #15240 ) ;
#19223 = CARTESIAN_POINT ( 'NONE',  ( 54.13287192849671214, 48.70051614449766220, -5.649768623646139964 ) ) ;
#19224 = CARTESIAN_POINT ( 'NONE',  ( -158.9999999999999716, -14.99999999999999645, 6.499999999999999112 ) ) ;
#19225 = DIRECTION ( 'NONE',  ( 0.000000000000000000, -0.000000000000000000, -1.000000000000000000 ) ) ;
#19226 = CARTESIAN_POINT ( 'NONE',  ( 19.02113032590300890, -13.81966011250085025, -9.000000000000000000 ) ) ;
#19227 = CARTESIAN_POINT ( 'NONE',  ( -4.000000000000000000, -2.512220745329312610, -3.469390707569719901 ) ) ;
#19228 = ORIENTED_EDGE ( 'NONE', *, *, #6754, .F. ) ;
#19229 = ORIENTED_EDGE ( 'NONE', *, *, #4838, .T. ) ;
#19230 = DIRECTION ( 'NONE',  ( -0.000000000000000000, 0.000000000000000000, -1.000000000000000000 ) ) ;
#19231 = LINE ( 'NONE', #19133, #12435 ) ;
#19232 = ORIENTED_EDGE ( 'NONE', *, *, #2763, .F. ) ;
#19233 = DIRECTION ( 'NONE',  ( -1.000000000000000000, -1.040834085586084257E-16, 0.000000000000000000 ) ) ;
#19234 = ORIENTED_EDGE ( 'NONE', *, *, #14413, .T. ) ;
#19235 = ORIENTED_EDGE ( 'NONE', *, *, #787, .T. ) ;
#19236 = EDGE_CURVE ( 'NONE', #13816, #16855, #7766, .T. ) ;
#19237 = CARTESIAN_POINT ( 'NONE',  ( 1.925929944387235853E-31, 15.00000000000001599, 15.00000000000000178 ) ) ;
#19238 = CARTESIAN_POINT ( 'NONE',  ( 3.880206590543186618, -3.396506438958517116, 1.117078279489015502 ) ) ;
#19239 = PRODUCT_RELATED_PRODUCT_CATEGORY ( 'part', '', ( #3649 ) ) ;
#19240 = CARTESIAN_POINT ( 'NONE',  ( 50.02271294988506156, 48.50051614449765935, -6.000000000000000888 ) ) ;
#19241 = DIRECTION ( 'NONE',  ( 0.000000000000000000, -1.224646799147353700E-16, 1.000000000000000000 ) ) ;
#19242 = EDGE_CURVE ( 'NONE', #10464, #15949, #10031, .T. ) ;
#19243 = VECTOR ( 'NONE', #4075, 1000.000000000000000 ) ;
#19244 = DIRECTION ( 'NONE',  ( 0.000000000000000000, 0.000000000000000000, 1.000000000000000000 ) ) ;
#19245 = CARTESIAN_POINT ( 'NONE',  ( 48.02776887271745210, 55.39948385550240317, -5.992620115222778487 ) ) ;
#19246 = DIRECTION ( 'NONE',  ( 0.000000000000000000, 0.000000000000000000, 1.000000000000000000 ) ) ;
#19247 = CARTESIAN_POINT ( 'NONE',  ( 43.34962307344081012, 54.89948385550240317, 2.184720259617164650 ) ) ;
#19248 = CARTESIAN_POINT ( 'NONE',  ( 43.18075615816994173, 49.80051614449765651, 4.924951120819380357 ) ) ;
#19249 = EDGE_CURVE ( 'NONE', #18471, #7311, #15315, .T. ) ;
#19250 = CARTESIAN_POINT ( 'NONE',  ( 4.132952817037859106, -2.031684012687264396, -3.518979934899745032 ) ) ;
#19251 = EDGE_CURVE ( 'NONE', #7579, #4866, #6304, .T. ) ;
#19252 = ORIENTED_EDGE ( 'NONE', *, *, #2329, .T. ) ;
#19253 = CARTESIAN_POINT ( 'NONE',  ( -54.99999999999996447, -14.99999999999998579, -15.00000000000000000 ) ) ;
#19254 = SHAPE_REPRESENTATION_RELATIONSHIP ( 'NONE' , 'NONE' ,  #6546, #9419 ) ;
#19255 = EDGE_CURVE ( 'NONE', #6843, #12831, #9513, .T. ) ;
#19256 = CARTESIAN_POINT ( 'NONE',  ( -154.9999999999999716, -14.99999999999999645, -15.00000000000000000 ) ) ;
#19257 = ORIENTED_EDGE ( 'NONE', *, *, #13276, .T. ) ;
#19258 = CARTESIAN_POINT ( 'NONE',  ( 6.534838248920899595, -2.951765777552420644, -5.112608298763837489 ) ) ;
#19259 = CIRCLE ( 'NONE', #17367, 15.00000000000000000 ) ;
#19260 = LINE ( 'NONE', #2968, #15648 ) ;
#19261 = AXIS2_PLACEMENT_3D ( 'NONE', #1493, #15116, #16404 ) ;
#19262 = EDGE_CURVE ( 'NONE', #17767, #12345, #16312, .T. ) ;
#19263 = CARTESIAN_POINT ( 'NONE',  ( 6.445127866599367650, -5.657054305385780246, -0.4229901806197432501 ) ) ;
#19264 = ADVANCED_FACE ( 'NONE', ( #6108 ), #13742, .T. ) ;
#19265 = CYLINDRICAL_SURFACE ( 'NONE', #12130, 5.000000000000000888 ) ;
#19266 = DIRECTION ( 'NONE',  ( 1.000000000000000000, 0.000000000000000000, 0.000000000000000000 ) ) ;
#19267 = CARTESIAN_POINT ( 'NONE',  ( 11.75570504584960041, -36.18033988749885310, -9.000000000000000000 ) ) ;
#19268 = CARTESIAN_POINT ( 'NONE',  ( -14.99999999999999822, -19.99999999999999645, -50.00000000000000000 ) ) ;
#19269 = B_SPLINE_CURVE_WITH_KNOTS ( 'NONE', 3,
 ( #3065, #6284, #6095, #19 ),
 .UNSPECIFIED., .F., .F.,
 ( 4, 4 ),
 ( 2.380739282773774244E-07, 0.002044882221487524104 ),
 .UNSPECIFIED. ) ;
#19270 = CARTESIAN_POINT ( 'NONE',  ( 56.65037692655918988, 51.89948385550241028, -2.184720259617163762 ) ) ;
#19271 = FACE_BOUND ( 'NONE', #13900, .T. ) ;
#19272 = CARTESIAN_POINT ( 'NONE',  ( 45.27934281921075410, 51.29948385550240175, -6.458785618021043895 ) ) ;
#19273 = CARTESIAN_POINT ( 'NONE',  ( 2.000000000000000000, -0.8865213383406694847, 1.535500000000001419 ) ) ;
#19274 = CARTESIAN_POINT ( 'NONE',  ( 55.94051828345053679, 49.20051614449766930, 4.345558710429044069 ) ) ;
#19275 = DIRECTION ( 'NONE',  ( 0.02857142857142857401, 0.9995917534020515305, -0.000000000000000000 ) ) ;
#19276 = CIRCLE ( 'NONE', #11395, 2.000000000000000000 ) ;
#19277 = ORIENTED_EDGE ( 'NONE', *, *, #5799, .T. ) ;
#19278 = B_SPLINE_CURVE_WITH_KNOTS ( 'NONE', 3,
 ( #6366, #9400, #1967, #486, #3529, #15478 ),
 .UNSPECIFIED., .F., .F.,
 ( 4, 2, 4 ),
 ( 0.005339748439308726613, 0.006800846765732536554, 0.008261945092156346496 ),
 .UNSPECIFIED. ) ;
#19279 = ORIENTED_EDGE ( 'NONE', *, *, #14173, .T. ) ;
#19280 = CARTESIAN_POINT ( 'NONE',  ( 12.54977455159135502, -35.57251292194776227, 9.000000000000000000 ) ) ;
#19281 = ORIENTED_EDGE ( 'NONE', *, *, #3350, .T. ) ;
#19282 =( GEOMETRIC_REPRESENTATION_CONTEXT ( 3 ) GLOBAL_UNCERTAINTY_ASSIGNED_CONTEXT ( ( #6544 ) ) GLOBAL_UNIT_ASSIGNED_CONTEXT ( ( #7590, #1811, #11897 ) ) REPRESENTATION_CONTEXT ( 'NONE', 'WORKASPACE' ) );
#19283 = FACE_BOUND ( 'NONE', #4382, .T. ) ;
#19284 = ORIENTED_EDGE ( 'NONE', *, *, #15020, .F. ) ;
#19285 = LINE ( 'NONE', #16422, #5352 ) ;
#19286 = ORIENTED_EDGE ( 'NONE', *, *, #13930, .T. ) ;
#19287 = AXIS2_PLACEMENT_3D ( 'NONE', #7616, #1181, #7156 ) ;
#19288 = DIRECTION ( 'NONE',  ( 1.000000000000000000, 0.000000000000000000, 0.000000000000000000 ) ) ;
#19289 = ORIENTED_EDGE ( 'NONE', *, *, #10698, .F. ) ;
#19290 = CARTESIAN_POINT ( 'NONE',  ( 58.41169779390614281, 57.99948385550241170, -0.02388180880523160798 ) ) ;
#19291 = AXIS2_PLACEMENT_3D ( 'NONE', #17756, #13530, #1676 ) ;
#19292 = DIRECTION ( 'NONE',  ( 0.000000000000000000, 0.000000000000000000, 1.000000000000000000 ) ) ;
#19293 = CARTESIAN_POINT ( 'NONE',  ( 44.30067958973596376, 58.89948385550241028, 1.875703265242204099 ) ) ;
#19294 = CARTESIAN_POINT ( 'NONE',  ( 1.149999999999998135, 4.959819536546779614E-16, 4.000000000000000000 ) ) ;
#19295 = EDGE_CURVE ( 'NONE', #4327, #508, #12223, .T. ) ;
#19296 = DIRECTION ( 'NONE',  ( -0.000000000000000000, -0.000000000000000000, 1.000000000000000000 ) ) ;
#19297 = CARTESIAN_POINT ( 'NONE',  ( 56.79116909180259398, 53.20051614449766220, 4.963592699178938972 ) ) ;
#19298 = AXIS2_PLACEMENT_3D ( 'NONE', #8735, #13246, #12949 ) ;
#19299 = CARTESIAN_POINT ( 'NONE',  ( 55.69932041026405045, 47.10051614449766078, 1.875703265242156359 ) ) ;
#19300 = DIRECTION ( 'NONE',  ( -1.000000000000000000, -0.000000000000000000, -0.000000000000000000 ) ) ;
#19301 = LINE ( 'NONE', #19402, #12204 ) ;
#19302 = ORIENTED_EDGE ( 'NONE', *, *, #406, .F. ) ;
#19303 = ORIENTED_EDGE ( 'NONE', *, *, #8713, .F. ) ;
#19304 = CYLINDRICAL_SURFACE ( 'NONE', #7487, 2.000000000000001776 ) ;
#19305 = ORIENTED_EDGE ( 'NONE', *, *, #10698, .T. ) ;
#19306 = EDGE_CURVE ( 'NONE', #9398, #11277, #12363, .T. ) ;
#19307 = CARTESIAN_POINT ( 'NONE',  ( 43.34962307344081012, 62.89948385550241028, 2.184720259617164650 ) ) ;
#19308 = CARTESIAN_POINT ( 'NONE',  ( -19.97007065299860784, -21.09374499507130452, 9.000000000000000000 ) ) ;
#19309 = ORIENTED_EDGE ( 'NONE', *, *, #10206, .T. ) ;
#19310 = DIRECTION ( 'NONE',  ( 0.000000000000000000, 0.000000000000000000, 1.000000000000000000 ) ) ;
#19311 = AXIS2_PLACEMENT_3D ( 'NONE', #1248, #5458, #5367 ) ;
#19312 = ADVANCED_FACE ( 'NONE', ( #4644 ), #16608, .T. ) ;
#19313 = CARTESIAN_POINT ( 'NONE',  ( 47.70284917648453415, 47.39948385550239607, -6.992620115222774047 ) ) ;
#19314 = ORIENTED_EDGE ( 'NONE', *, *, #16042, .F. ) ;
#19315 = CARTESIAN_POINT ( 'NONE',  ( -154.9999999999999716, -14.99999999999999645, 15.00000000000000000 ) ) ;
#19316 = ORIENTED_EDGE ( 'NONE', *, *, #13576, .T. ) ;
#19317 = CARTESIAN_POINT ( 'NONE',  ( -3.522875095019672109, 2.820352903225427532, -3.598441714920591394 ) ) ;
#19318 = CARTESIAN_POINT ( 'NONE',  ( 44.03140696652192787, 55.19948385550238612, -4.306917132069425058 ) ) ;
#19319 =( GEOMETRIC_REPRESENTATION_CONTEXT ( 3 ) GLOBAL_UNCERTAINTY_ASSIGNED_CONTEXT ( ( #496 ) ) GLOBAL_UNIT_ASSIGNED_CONTEXT ( ( #5087, #17061, #7831 ) ) REPRESENTATION_CONTEXT ( 'NONE', 'WORKASPACE' ) );
#19320 = PLANE ( 'NONE',  #9912 ) ;
#19321 = CARTESIAN_POINT ( 'NONE',  ( 56.65037692655921120, 45.10051614449766078, 2.184720259617097593 ) ) ;
#19322 = DIRECTION ( 'NONE',  ( -0.000000000000000000, 1.000000000000000000, -0.000000000000000000 ) ) ;
#19323 =( LENGTH_UNIT ( ) NAMED_UNIT ( * ) SI_UNIT ( .MILLI., .METRE. ) );
#19324 = CARTESIAN_POINT ( 'NONE',  ( -4.000000000000000000, 1.677772373332757194, -3.535253723897187506 ) ) ;
#19325 = ORIENTED_EDGE ( 'NONE', *, *, #1640, .F. ) ;
#19326 = AXIS2_PLACEMENT_3D ( 'NONE', #8595, #10155, #8394 ) ;
#19327 = ORIENTED_EDGE ( 'NONE', *, *, #5259, .T. ) ;
#19328 = ORIENTED_EDGE ( 'NONE', *, *, #15402, .F. ) ;
#19329 = DIRECTION ( 'NONE',  ( -1.000000000000000000, 0.000000000000000000, 0.000000000000000000 ) ) ;
#19330 = FILL_AREA_STYLE_COLOUR ( '', #15607 ) ;
#19331 = CARTESIAN_POINT ( 'NONE',  ( 42.63976443033212860, 46.99948385550240459, 0.02388180880522514787 ) ) ;
#19332 = VECTOR ( 'NONE', #5885, 1000.000000000000000 ) ;
#19333 = DIRECTION ( 'NONE',  ( -0.000000000000000000, -0.000000000000000000, -1.000000000000000000 ) ) ;
#19334 = VERTEX_POINT ( 'NONE', #1990 ) ;
#19335 = CARTESIAN_POINT ( 'NONE',  ( 3.098410542199072637, -7.060458129626440815, -1.000000000000000000 ) ) ;
#19336 = ORIENTED_EDGE ( 'NONE', *, *, #10821, .T. ) ;
#19337 = VERTEX_POINT ( 'NONE', #13921 ) ;
#19338 = DIRECTION ( 'NONE',  ( -1.000000000000000000, 0.000000000000000000, 0.000000000000000000 ) ) ;
#19339 = UNCERTAINTY_MEASURE_WITH_UNIT (LENGTH_MEASURE( 1.000000000000000082E-05 ), #8900, 'distance_accuracy_value', 'NONE');
#19340 = DIRECTION ( 'NONE',  ( -1.000000000000000000, 0.000000000000000000, 0.000000000000000000 ) ) ;
#19341 = CARTESIAN_POINT ( 'NONE',  ( 48.07319477248762496, 50.40051614449766504, -6.007379884777208190 ) ) ;
#19342 = FACE_OUTER_BOUND ( 'NONE', #18896, .T. ) ;
#19343 = PRODUCT_DEFINITION_SHAPE ( 'NONE', 'NONE',  #6264 ) ;
#19344 = DIRECTION ( 'NONE',  ( 1.000000000000000000, 0.000000000000000000, 0.000000000000000000 ) ) ;
#19345 = CARTESIAN_POINT ( 'NONE',  ( 51.97223112728254790, 56.39948385550241028, 5.992620115222778487 ) ) ;
#19346 = CARTESIAN_POINT ( 'NONE',  ( 2.725741868436127202, -3.045094352033990148, -3.220599429844051453 ) ) ;
#19347 = CARTESIAN_POINT ( 'NONE',  ( 47.70284917648453415, 55.39948385550238896, -6.992620115222774047 ) ) ;
#19348 = CARTESIAN_POINT ( 'NONE',  ( 43.20883090819742023, 56.20051614449766220, -4.963592699178938972 ) ) ;
#19349 = CARTESIAN_POINT ( 'NONE',  ( 4.082498951862917558, -2.020725942163694722, -3.499999999999999556 ) ) ;
#19350 = AXIS2_PLACEMENT_3D ( 'NONE', #16424, #3654, #13751 ) ;
#19351 = LINE ( 'NONE', #1479, #2742 ) ;
#19352 = DIRECTION ( 'NONE',  ( 1.000000000000000000, 0.000000000000000000, 0.000000000000000000 ) ) ;
#19353 =( NAMED_UNIT ( * ) SI_UNIT ( $, .STERADIAN. ) SOLID_ANGLE_UNIT ( ) );
#19354 = VECTOR ( 'NONE', #2051, 1000.000000000000000 ) ;
#19355 = EDGE_CURVE ( 'NONE', #15389, #16193, #7846, .T. ) ;
#19356 = DIRECTION ( 'NONE',  ( 5.551115123125782702E-17, 0.000000000000000000, -1.000000000000000000 ) ) ;
#19357 = SHAPE_REPRESENTATION ( 'motor', ( #10359 ), #13801 ) ;
#19358 = ORIENTED_EDGE ( 'NONE', *, *, #6450, .F. ) ;
#19359 = CARTESIAN_POINT ( 'NONE',  ( -4.140404888673278272, -2.228338276487456415, -3.686887068327035166 ) ) ;
#19360 = CIRCLE ( 'NONE', #2747, 1.000000000000000666 ) ;
#19361 = PRODUCT_DEFINITION_SHAPE ( 'NONE', 'NONE',  #19440 ) ;
#19362 = FACE_OUTER_BOUND ( 'NONE', #17406, .T. ) ;
#19363 = VECTOR ( 'NONE', #7246, 1000.000000000000000 ) ;
#19364 = CARTESIAN_POINT ( 'NONE',  ( -155.0777214229742071, -18.79920509849242549, 15.00000000000000000 ) ) ;
#19365 = CARTESIAN_POINT ( 'NONE',  ( 32.00000000000000000, 1.000000000000000000, -5.999999999999998224 ) ) ;
#19366 = DIRECTION ( 'NONE',  ( 1.000000000000000000, 0.000000000000000000, 0.000000000000000000 ) ) ;
#19367 = CYLINDRICAL_SURFACE ( 'NONE', #14217, 1.000000000000000888 ) ;
#19368 = DIRECTION ( 'NONE',  ( 0.000000000000000000, 0.000000000000000000, 1.000000000000000000 ) ) ;
#19369 = CARTESIAN_POINT ( 'NONE',  ( 55.94051828345050836, 55.79948385550238044, -4.345558710429104465 ) ) ;
#19370 = EDGE_CURVE ( 'NONE', #440, #6090, #12852, .T. ) ;
#19371 = CARTESIAN_POINT ( 'NONE',  ( 4.000000000000000000, 2.309401076758497151, -3.433295621305379353 ) ) ;
#19372 = CARTESIAN_POINT ( 'NONE',  ( 49.97728705011486738, 55.49948385550241170, -8.000000000000001776 ) ) ;
#19373 = CARTESIAN_POINT ( 'NONE',  ( 75.00000000000001421, -39.99999999999998579, -20.00000000000000000 ) ) ;
#19374 = CARTESIAN_POINT ( 'NONE',  ( 52.25172492374527877, 47.40051614449766504, 7.007379884777203749 ) ) ;
#19375 = VECTOR ( 'NONE', #319, 1000.000000000000114 ) ;
#19376 = DIRECTION ( 'NONE',  ( -1.000000000000000000, -0.000000000000000000, -0.000000000000000000 ) ) ;
#19378 = ORIENTED_EDGE ( 'NONE', *, *, #12398, .F. ) ;
#19377 = EDGE_CURVE ( 'NONE', #16030, #8220, #6588, .T. ) ;
#19379 = EDGE_CURVE ( 'NONE', #9229, #3704, #9104, .T. ) ;
#19380 = ORIENTED_EDGE ( 'NONE', *, *, #3081, .F. ) ;
#19381 = DIRECTION ( 'NONE',  ( 0.000000000000000000, 0.000000000000000000, 1.000000000000000000 ) ) ;
#19382 = ORIENTED_EDGE ( 'NONE', *, *, #6502, .T. ) ;
#19383 = DIRECTION ( 'NONE',  ( -1.000000000000000000, 0.000000000000000000, 0.000000000000000000 ) ) ;
#19384 = ORIENTED_EDGE ( 'NONE', *, *, #5545, .T. ) ;
#19385 = DIRECTION ( 'NONE',  ( -1.000000000000000000, -0.000000000000000000, -0.000000000000000000 ) ) ;
#19386 = ADVANCED_FACE ( 'NONE', ( #16001 ), #6968, .T. ) ;
#19387 = EDGE_LOOP ( 'NONE', ( #899, #15727 ) ) ;
#19388 = ADVANCED_FACE ( 'NONE', ( #17379 ), #6578, .T. ) ;
#19389 = DIRECTION ( 'NONE',  ( 0.000000000000000000, 0.000000000000000000, -1.000000000000000000 ) ) ;
#19390 = VERTEX_POINT ( 'NONE', #9898 ) ;
#19391 = CARTESIAN_POINT ( 'NONE',  ( 2.000000000000000000, -0.8865213383406694847, 1.535500000000001419 ) ) ;
#19392 = CIRCLE ( 'NONE', #14974, 0.2000000000000000944 ) ;
#19393 = DIRECTION ( 'NONE',  ( 1.000000000000000000, 0.000000000000000000, 0.000000000000000000 ) ) ;
#19394 = AXIS2_PLACEMENT_3D ( 'NONE', #16465, #7626, #3509 ) ;
#19395 = CARTESIAN_POINT ( 'NONE',  ( 55.69932041026404335, 57.89948385550241028, -1.875703265242203432 ) ) ;
#19396 = EDGE_CURVE ( 'NONE', #13178, #12683, #16323, .T. ) ;
#19397 = CARTESIAN_POINT ( 'NONE',  ( 20.00000000000000000, -20.00000000000000000, -23.00000000000000000 ) ) ;
#19398 = CARTESIAN_POINT ( 'NONE',  ( 3.160591952521659032, -3.281206521718069258, -0.8000000000000000444 ) ) ;
#19399 = CARTESIAN_POINT ( 'NONE',  ( 57.61547081786810764, 54.90051614449765793, -2.450534656007114176 ) ) ;
#19400 = CARTESIAN_POINT ( 'NONE',  ( 44.91013252490150620, 46.20051614449766220, -3.727524721679154940 ) ) ;
#19401 = DIRECTION ( 'NONE',  ( 0.000000000000000000, 0.000000000000000000, 1.000000000000000000 ) ) ;
#19402 = CARTESIAN_POINT ( 'NONE',  ( 3.129923130707922496, -23.63917314727666152, -9.999999999999994671 ) ) ;
#19403 = ORIENTED_EDGE ( 'NONE', *, *, #4858, .T. ) ;
#19404 = ORIENTED_EDGE ( 'NONE', *, *, #3457, .F. ) ;
#19405 = CARTESIAN_POINT ( 'NONE',  ( -151.2001253019789431, -14.96914097636792818, 15.79999999999999893 ) ) ;
#19406 = ORIENTED_EDGE ( 'NONE', *, *, #4848, .F. ) ;
#19407 = AXIS2_PLACEMENT_3D ( 'NONE', #15763, #2342, #12712 ) ;
#19408 = CIRCLE ( 'NONE', #7476, 0.1000000000000011297 ) ;
#19409 = DIRECTION ( 'NONE',  ( -0.000000000000000000, -0.000000000000000000, 1.000000000000000000 ) ) ;
#19410 = CARTESIAN_POINT ( 'NONE',  ( 19.30627432446641123, -14.77814480204120784, -9.000000000000000000 ) ) ;
#19411 = EDGE_LOOP ( 'NONE', ( #10537, #6416 ) ) ;
#19412 = DIRECTION ( 'NONE',  ( 0.000000000000000000, 0.000000000000000000, -1.000000000000000000 ) ) ;
#19413 = DIRECTION ( 'NONE',  ( 0.000000000000000000, -0.000000000000000000, 1.000000000000000000 ) ) ;
#19414 = ORIENTED_EDGE ( 'NONE', *, *, #13165, .T. ) ;
#19415 =( GEOMETRIC_REPRESENTATION_CONTEXT ( 3 ) GLOBAL_UNCERTAINTY_ASSIGNED_CONTEXT ( ( #16180 ) ) GLOBAL_UNIT_ASSIGNED_CONTEXT ( ( #2564, #13024, #10267 ) ) REPRESENTATION_CONTEXT ( 'NONE', 'WORKASPACE' ) );
#19416 = ORIENTED_EDGE ( 'NONE', *, *, #18751, .T. ) ;
#19417 = NEXT_ASSEMBLY_USAGE_OCCURRENCE ( 'NAUO1', ' ', ' ', #3046, #17058, $ ) ;
#19418 = NEXT_ASSEMBLY_USAGE_OCCURRENCE ( 'NAUO2', ' ', ' ', #3046, #10089, $ ) ;
#19419 = NEXT_ASSEMBLY_USAGE_OCCURRENCE ( 'NAUO3', ' ', ' ', #3046, #1359, $ ) ;
#19420 = NEXT_ASSEMBLY_USAGE_OCCURRENCE ( 'NAUO4', ' ', ' ', #3046, #6612, $ ) ;
#19421 = NEXT_ASSEMBLY_USAGE_OCCURRENCE ( 'NAUO5', ' ', ' ', #3046, #5304, $ ) ;
#19422 = NEXT_ASSEMBLY_USAGE_OCCURRENCE ( 'NAUO6', ' ', ' ', #3046, #3281, $ ) ;
#19423 = NEXT_ASSEMBLY_USAGE_OCCURRENCE ( 'NAUO7', ' ', ' ', #3046, #6742, $ ) ;
#19424 = NEXT_ASSEMBLY_USAGE_OCCURRENCE ( 'NAUO8', ' ', ' ', #3046, #6742, $ ) ;
#19425 = NEXT_ASSEMBLY_USAGE_OCCURRENCE ( 'NAUO9', ' ', ' ', #3046, #8787, $ ) ;
#19426 = NEXT_ASSEMBLY_USAGE_OCCURRENCE ( 'NAUO10', ' ', ' ', #3046, #160, $ ) ;
#19427 = NEXT_ASSEMBLY_USAGE_OCCURRENCE ( 'NAUO11', ' ', ' ', #3046, #160, $ ) ;
#19428 = NEXT_ASSEMBLY_USAGE_OCCURRENCE ( 'NAUO12', ' ', ' ', #3046, #14639, $ ) ;
#19429 = NEXT_ASSEMBLY_USAGE_OCCURRENCE ( 'NAUO13', ' ', ' ', #3046, #14639, $ ) ;
#19430 = NEXT_ASSEMBLY_USAGE_OCCURRENCE ( 'NAUO14', ' ', ' ', #3046, #10570, $ ) ;
#19431 = NEXT_ASSEMBLY_USAGE_OCCURRENCE ( 'NAUO15', ' ', ' ', #3046, #10570, $ ) ;
#19432 = NEXT_ASSEMBLY_USAGE_OCCURRENCE ( 'NAUO16', ' ', ' ', #3046, #10209, $ ) ;
#19433 = NEXT_ASSEMBLY_USAGE_OCCURRENCE ( 'NAUO17', ' ', ' ', #3046, #6264, $ ) ;
#19434 = NEXT_ASSEMBLY_USAGE_OCCURRENCE ( 'NAUO18', ' ', ' ', #3046, #9726, $ ) ;
#19435 = NEXT_ASSEMBLY_USAGE_OCCURRENCE ( 'NAUO19', ' ', ' ', #3046, #12013, $ ) ;
#19436 = NEXT_ASSEMBLY_USAGE_OCCURRENCE ( 'NAUO20', ' ', ' ', #3046, #12013, $ ) ;
#19437 = NEXT_ASSEMBLY_USAGE_OCCURRENCE ( 'NAUO21', ' ', ' ', #3046, #13215, $ ) ;
#19438 = NEXT_ASSEMBLY_USAGE_OCCURRENCE ( 'NAUO22', ' ', ' ', #3046, #13215, $ ) ;
#19439 = NEXT_ASSEMBLY_USAGE_OCCURRENCE ( 'NAUO23', ' ', ' ', #3046, #160, $ ) ;
#19440 = NEXT_ASSEMBLY_USAGE_OCCURRENCE ( 'NAUO24', ' ', ' ', #3046, #10570, $ ) ;
#19441=COLOUR_RGB('Dark Blue',0.08,0.2,0.34);
#19442=FILL_AREA_STYLE_COLOUR('',#19441);
#19443=FILL_AREA_STYLE('',(#19442));
#19444=SURFACE_STYLE_FILL_AREA(#19443);
#19445=SURFACE_SIDE_STYLE('',(#19444));
#19446=SURFACE_STYLE_USAGE(.BOTH.,#19445);
#19447=PRESENTATION_STYLE_ASSIGNMENT((#19446));
#19448=COLOUR_RGB('Light Blue',0.38,0.62,0.78);
#19449=FILL_AREA_STYLE_COLOUR('',#19448);
#19450=FILL_AREA_STYLE('',(#19449));
#19451=SURFACE_STYLE_FILL_AREA(#19450);
#19452=SURFACE_SIDE_STYLE('',(#19451));
#19453=SURFACE_STYLE_USAGE(.BOTH.,#19452);
#19454=PRESENTATION_STYLE_ASSIGNMENT((#19453));
#19455=COLOUR_RGB('Sky Blue',0.24,0.69,0.87);
#19456=FILL_AREA_STYLE_COLOUR('',#19455);
#19457=FILL_AREA_STYLE('',(#19456));
#19458=SURFACE_STYLE_FILL_AREA(#19457);
#19459=SURFACE_SIDE_STYLE('',(#19458));
#19460=SURFACE_STYLE_USAGE(.BOTH.,#19459);
#19461=PRESENTATION_STYLE_ASSIGNMENT((#19460));
#19462=COLOUR_RGB('Grey',0.48,0.52,0.57);
#19463=FILL_AREA_STYLE_COLOUR('',#19462);
#19464=FILL_AREA_STYLE('',(#19463));
#19465=SURFACE_STYLE_FILL_AREA(#19464);
#19466=SURFACE_SIDE_STYLE('',(#19465));
#19467=SURFACE_STYLE_USAGE(.BOTH.,#19466);
#19468=PRESENTATION_STYLE_ASSIGNMENT((#19467));
#19469=COLOUR_RGB('Black',0.12,0.14,0.17);
#19470=FILL_AREA_STYLE_COLOUR('',#19469);
#19471=FILL_AREA_STYLE('',(#19470));
#19472=SURFACE_STYLE_FILL_AREA(#19471);
#19473=SURFACE_SIDE_STYLE('',(#19472));
#19474=SURFACE_STYLE_USAGE(.BOTH.,#19473);
#19475=PRESENTATION_STYLE_ASSIGNMENT((#19474));
#19476=COLOUR_RGB('Off White',0.89,0.88,0.83);
#19477=FILL_AREA_STYLE_COLOUR('',#19476);
#19478=FILL_AREA_STYLE('',(#19477));
#19479=SURFACE_STYLE_FILL_AREA(#19478);
#19480=SURFACE_SIDE_STYLE('',(#19479));
#19481=SURFACE_STYLE_USAGE(.BOTH.,#19480);
#19482=PRESENTATION_STYLE_ASSIGNMENT((#19481));
ENDSEC;
END-ISO-10303-21;
